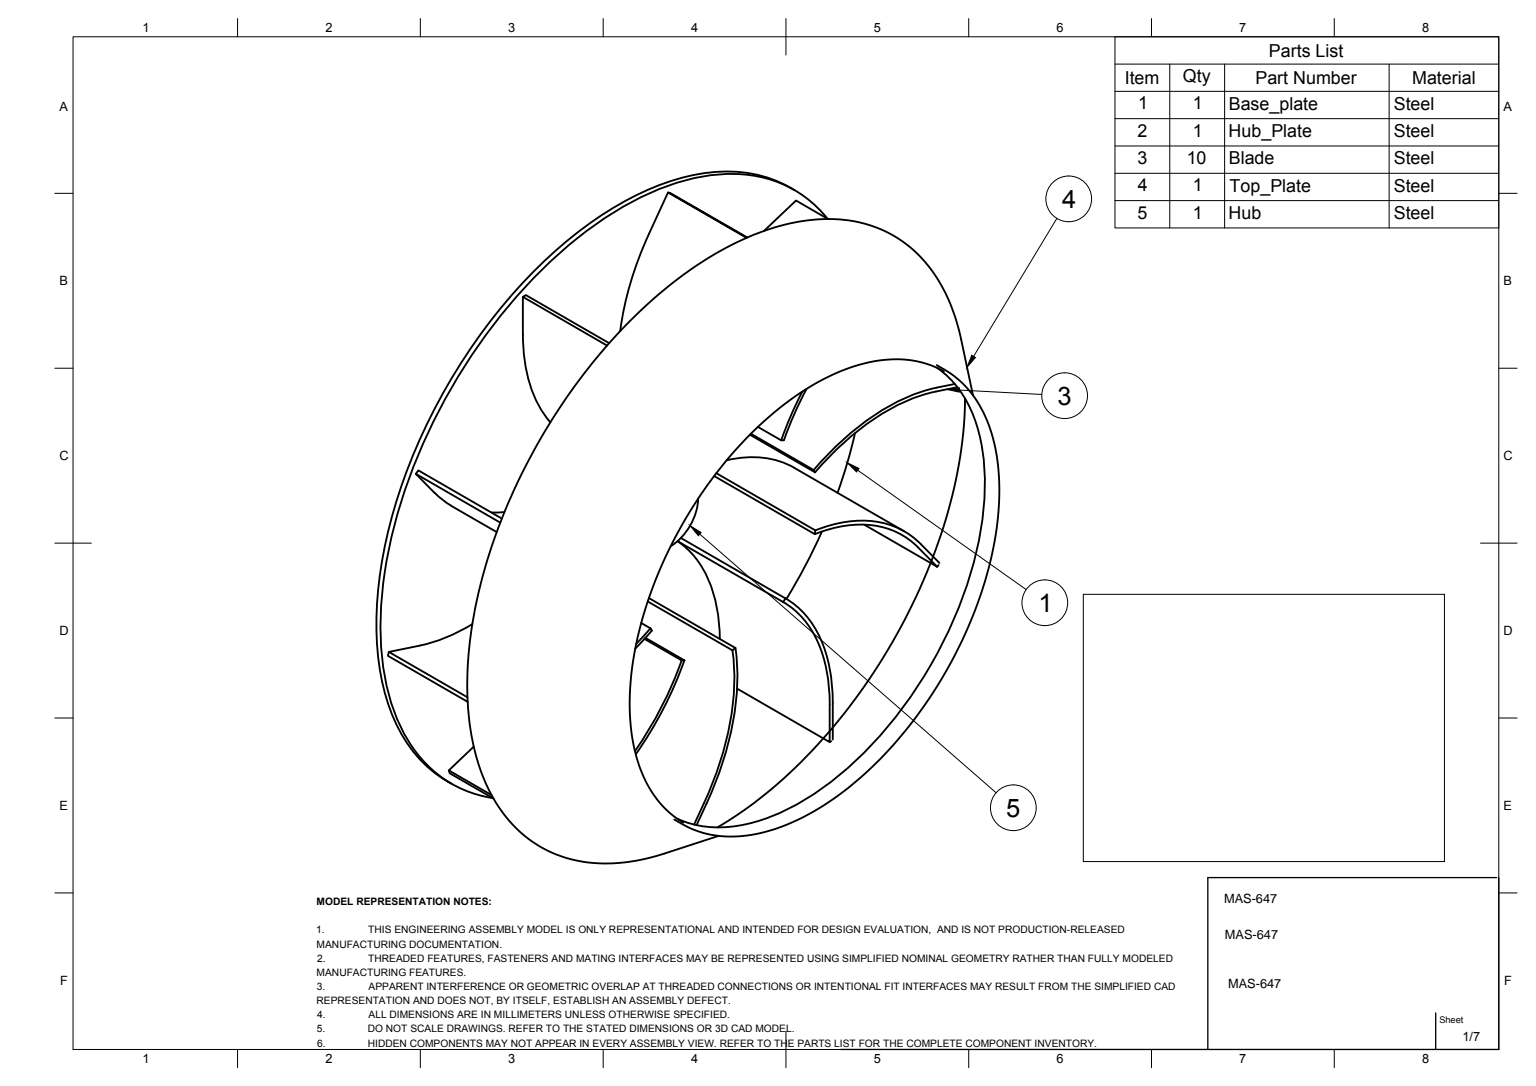
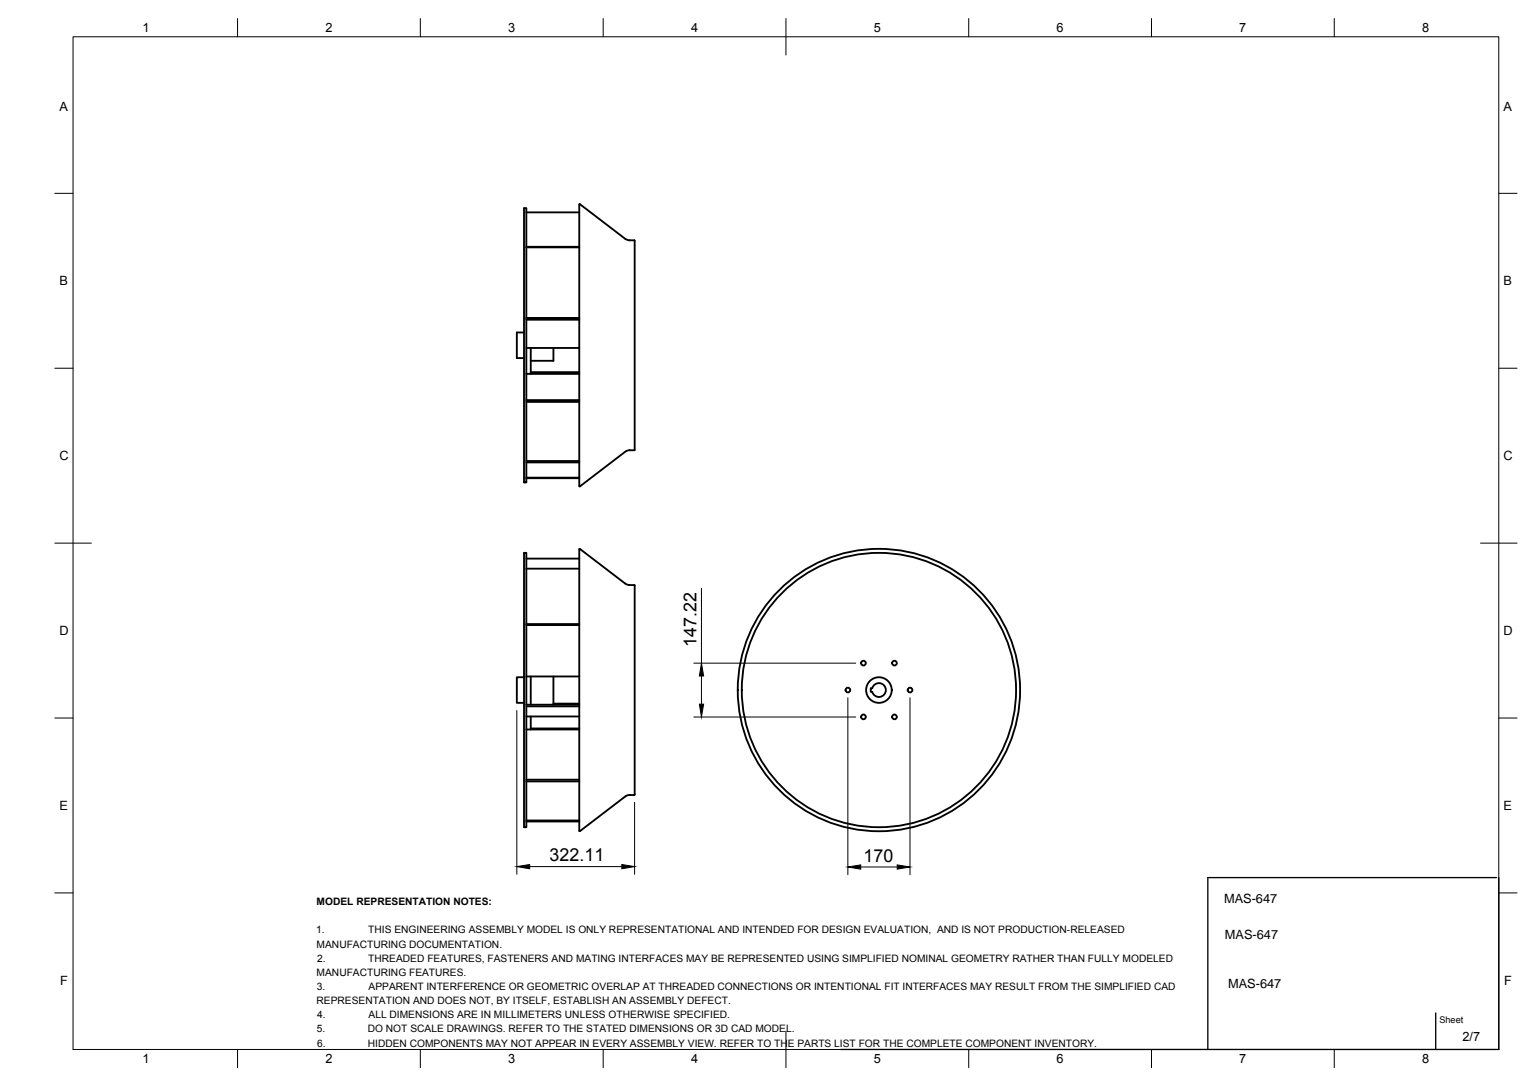
ISO-10303-21;
HEADER;
FILE_DESCRIPTION((''),'2;1');
FILE_NAME('MAS-647','2026-10-09T11:36:02-07:00',(''),(''),'','','');
FILE_SCHEMA (('AUTOMOTIVE_DESIGN { 1 0 10303 214 3 1 1 }'));
ENDSEC;
DATA;
#10 = MECHANICAL_DESIGN_GEOMETRIC_PRESENTATION_REPRESENTATION('',(#82,#83,
#84,#85,#86),#1549) ;
#11 = ITEM_DEFINED_TRANSFORMATION($,$,#906,#1009) ;
#12 = ITEM_DEFINED_TRANSFORMATION($,$,#933,#1010) ;
#13 = ITEM_DEFINED_TRANSFORMATION($,$,#994,#1011) ;
#14 = ITEM_DEFINED_TRANSFORMATION($,$,#960,#1012) ;
#15 = ITEM_DEFINED_TRANSFORMATION($,$,#978,#1013) ;
#16 = ITEM_DEFINED_TRANSFORMATION($,$,#994,#1014) ;
#17 = ITEM_DEFINED_TRANSFORMATION($,$,#994,#1015) ;
#18 = ITEM_DEFINED_TRANSFORMATION($,$,#994,#1016) ;
#19 = ITEM_DEFINED_TRANSFORMATION($,$,#994,#1017) ;
#20 = ITEM_DEFINED_TRANSFORMATION($,$,#994,#1018) ;
#21 = ITEM_DEFINED_TRANSFORMATION($,$,#994,#1019) ;
#22 = ITEM_DEFINED_TRANSFORMATION($,$,#994,#1020) ;
#23 = ITEM_DEFINED_TRANSFORMATION($,$,#994,#1021) ;
#24 = ITEM_DEFINED_TRANSFORMATION($,$,#994,#1022) ;
#25 = (
REPRESENTATION_RELATIONSHIP($,$,#1581,#1580)
REPRESENTATION_RELATIONSHIP_WITH_TRANSFORMATION(#11)
SHAPE_REPRESENTATION_RELATIONSHIP()
) ;
#26 = (
REPRESENTATION_RELATIONSHIP($,$,#1582,#1580)
REPRESENTATION_RELATIONSHIP_WITH_TRANSFORMATION(#12)
SHAPE_REPRESENTATION_RELATIONSHIP()
) ;
#27 = (
REPRESENTATION_RELATIONSHIP($,$,#1585,#1580)
REPRESENTATION_RELATIONSHIP_WITH_TRANSFORMATION(#13)
SHAPE_REPRESENTATION_RELATIONSHIP()
) ;
#28 = (
REPRESENTATION_RELATIONSHIP($,$,#1583,#1580)
REPRESENTATION_RELATIONSHIP_WITH_TRANSFORMATION(#14)
SHAPE_REPRESENTATION_RELATIONSHIP()
) ;
#29 = (
REPRESENTATION_RELATIONSHIP($,$,#1584,#1580)
REPRESENTATION_RELATIONSHIP_WITH_TRANSFORMATION(#15)
SHAPE_REPRESENTATION_RELATIONSHIP()
) ;
#30 = (
REPRESENTATION_RELATIONSHIP($,$,#1585,#1580)
REPRESENTATION_RELATIONSHIP_WITH_TRANSFORMATION(#16)
SHAPE_REPRESENTATION_RELATIONSHIP()
) ;
#31 = (
REPRESENTATION_RELATIONSHIP($,$,#1585,#1580)
REPRESENTATION_RELATIONSHIP_WITH_TRANSFORMATION(#17)
SHAPE_REPRESENTATION_RELATIONSHIP()
) ;
#32 = (
REPRESENTATION_RELATIONSHIP($,$,#1585,#1580)
REPRESENTATION_RELATIONSHIP_WITH_TRANSFORMATION(#18)
SHAPE_REPRESENTATION_RELATIONSHIP()
) ;
#33 = (
REPRESENTATION_RELATIONSHIP($,$,#1585,#1580)
REPRESENTATION_RELATIONSHIP_WITH_TRANSFORMATION(#19)
SHAPE_REPRESENTATION_RELATIONSHIP()
) ;
#34 = (
REPRESENTATION_RELATIONSHIP($,$,#1585,#1580)
REPRESENTATION_RELATIONSHIP_WITH_TRANSFORMATION(#20)
SHAPE_REPRESENTATION_RELATIONSHIP()
) ;
#35 = (
REPRESENTATION_RELATIONSHIP($,$,#1585,#1580)
REPRESENTATION_RELATIONSHIP_WITH_TRANSFORMATION(#21)
SHAPE_REPRESENTATION_RELATIONSHIP()
) ;
#36 = (
REPRESENTATION_RELATIONSHIP($,$,#1585,#1580)
REPRESENTATION_RELATIONSHIP_WITH_TRANSFORMATION(#22)
SHAPE_REPRESENTATION_RELATIONSHIP()
) ;
#37 = (
REPRESENTATION_RELATIONSHIP($,$,#1585,#1580)
REPRESENTATION_RELATIONSHIP_WITH_TRANSFORMATION(#23)
SHAPE_REPRESENTATION_RELATIONSHIP()
) ;
#38 = (
REPRESENTATION_RELATIONSHIP($,$,#1585,#1580)
REPRESENTATION_RELATIONSHIP_WITH_TRANSFORMATION(#24)
SHAPE_REPRESENTATION_RELATIONSHIP()
) ;
#39 = CONTEXT_DEPENDENT_SHAPE_REPRESENTATION(#25,#1566) ;
#40 = CONTEXT_DEPENDENT_SHAPE_REPRESENTATION(#26,#1567) ;
#41 = CONTEXT_DEPENDENT_SHAPE_REPRESENTATION(#27,#1568) ;
#42 = CONTEXT_DEPENDENT_SHAPE_REPRESENTATION(#28,#1569) ;
#43 = CONTEXT_DEPENDENT_SHAPE_REPRESENTATION(#29,#1570) ;
#44 = CONTEXT_DEPENDENT_SHAPE_REPRESENTATION(#30,#1571) ;
#45 = CONTEXT_DEPENDENT_SHAPE_REPRESENTATION(#31,#1572) ;
#46 = CONTEXT_DEPENDENT_SHAPE_REPRESENTATION(#32,#1573) ;
#47 = CONTEXT_DEPENDENT_SHAPE_REPRESENTATION(#33,#1574) ;
#48 = CONTEXT_DEPENDENT_SHAPE_REPRESENTATION(#34,#1575) ;
#49 = CONTEXT_DEPENDENT_SHAPE_REPRESENTATION(#35,#1576) ;
#50 = CONTEXT_DEPENDENT_SHAPE_REPRESENTATION(#36,#1577) ;
#51 = CONTEXT_DEPENDENT_SHAPE_REPRESENTATION(#37,#1578) ;
#52 = CONTEXT_DEPENDENT_SHAPE_REPRESENTATION(#38,#1579) ;
#53 = NEXT_ASSEMBLY_USAGE_OCCURRENCE('Base_Plate:1','Base_Plate:1',
'Base_Plate:1',#1587,#1588,'Base_Plate:1') ;
#54 = NEXT_ASSEMBLY_USAGE_OCCURRENCE('Hub_Plate:1','Hub_Plate:1',
'Hub_Plate:1',#1587,#1589,'Hub_Plate:1') ;
#55 = NEXT_ASSEMBLY_USAGE_OCCURRENCE('Blade:1','Blade:1','Blade:1',#1587,
#1592,'Blade:1') ;
#56 = NEXT_ASSEMBLY_USAGE_OCCURRENCE('Top_Plate:1','Top_Plate:1',
'Top_Plate:1',#1587,#1590,'Top_Plate:1') ;
#57 = NEXT_ASSEMBLY_USAGE_OCCURRENCE('Hub:1','Hub:1','Hub:1',#1587,#1591,
'Hub:1') ;
#58 = NEXT_ASSEMBLY_USAGE_OCCURRENCE('Blade:2','Blade:2','Blade:2',#1587,
#1592,'Blade:2') ;
#59 = NEXT_ASSEMBLY_USAGE_OCCURRENCE('Blade:3','Blade:3','Blade:3',#1587,
#1592,'Blade:3') ;
#60 = NEXT_ASSEMBLY_USAGE_OCCURRENCE('Blade:4','Blade:4','Blade:4',#1587,
#1592,'Blade:4') ;
#61 = NEXT_ASSEMBLY_USAGE_OCCURRENCE('Blade:5','Blade:5','Blade:5',#1587,
#1592,'Blade:5') ;
#62 = NEXT_ASSEMBLY_USAGE_OCCURRENCE('Blade:6','Blade:6','Blade:6',#1587,
#1592,'Blade:6') ;
#63 = NEXT_ASSEMBLY_USAGE_OCCURRENCE('Blade:7','Blade:7','Blade:7',#1587,
#1592,'Blade:7') ;
#64 = NEXT_ASSEMBLY_USAGE_OCCURRENCE('Blade:8','Blade:8','Blade:8',#1587,
#1592,'Blade:8') ;
#65 = NEXT_ASSEMBLY_USAGE_OCCURRENCE('Blade:9','Blade:9','Blade:9',#1587,
#1592,'Blade:9') ;
#66 = NEXT_ASSEMBLY_USAGE_OCCURRENCE('Blade:10','Blade:10','Blade:10',#1587,
#1592,'Blade:10') ;
#67 = CONICAL_SURFACE('',#965,384.29203539823,0.652265221120532) ;
#68 = CONICAL_SURFACE('',#974,287.,0.652265221120532) ;
#69 = TOROIDAL_SURFACE('',#961,307.,20.) ;
#70 = TOROIDAL_SURFACE('',#970,286.,1.) ;
#71 = TOROIDAL_SURFACE('',#976,385.086746274481,0.99999999999999) ;
#72 = SHAPE_REPRESENTATION_RELATIONSHIP('SRR','None',#1581,#77) ;
#73 = SHAPE_REPRESENTATION_RELATIONSHIP('SRR','None',#1582,#78) ;
#74 = SHAPE_REPRESENTATION_RELATIONSHIP('SRR','None',#1583,#79) ;
#75 = SHAPE_REPRESENTATION_RELATIONSHIP('SRR','None',#1584,#80) ;
#76 = SHAPE_REPRESENTATION_RELATIONSHIP('SRR','None',#1585,#81) ;
#77 = ADVANCED_BREP_SHAPE_REPRESENTATION('',(#87),#1544) ;
#78 = ADVANCED_BREP_SHAPE_REPRESENTATION('',(#88),#1545) ;
#79 = ADVANCED_BREP_SHAPE_REPRESENTATION('',(#89),#1546) ;
#80 = ADVANCED_BREP_SHAPE_REPRESENTATION('',(#90),#1547) ;
#81 = ADVANCED_BREP_SHAPE_REPRESENTATION('',(#91),#1548) ;
#82 = STYLED_ITEM('',(#1615),#87) ;
#83 = STYLED_ITEM('',(#1615),#88) ;
#84 = STYLED_ITEM('',(#1615),#89) ;
#85 = STYLED_ITEM('',(#1615),#90) ;
#86 = STYLED_ITEM('',(#1615),#91) ;
#87 = MANIFOLD_SOLID_BREP('Body1',#844) ;
#88 = MANIFOLD_SOLID_BREP('Body1',#845) ;
#89 = MANIFOLD_SOLID_BREP('Body1',#846) ;
#90 = MANIFOLD_SOLID_BREP('Body1',#847) ;
#91 = MANIFOLD_SOLID_BREP('Body1',#848) ;
#92 = FACE_BOUND('',#196,.T.) ;
#93 = FACE_BOUND('',#197,.T.) ;
#94 = FACE_BOUND('',#198,.T.) ;
#95 = FACE_BOUND('',#199,.T.) ;
#96 = FACE_BOUND('',#200,.T.) ;
#97 = FACE_BOUND('',#201,.T.) ;
#98 = FACE_BOUND('',#202,.T.) ;
#99 = FACE_BOUND('',#204,.T.) ;
#100 = FACE_BOUND('',#205,.T.) ;
#101 = FACE_BOUND('',#206,.T.) ;
#102 = FACE_BOUND('',#207,.T.) ;
#103 = FACE_BOUND('',#208,.T.) ;
#104 = FACE_BOUND('',#209,.T.) ;
#105 = FACE_BOUND('',#210,.T.) ;
#106 = FACE_BOUND('',#220,.T.) ;
#107 = FACE_BOUND('',#221,.T.) ;
#108 = FACE_BOUND('',#222,.T.) ;
#109 = FACE_BOUND('',#223,.T.) ;
#110 = FACE_BOUND('',#224,.T.) ;
#111 = FACE_BOUND('',#225,.T.) ;
#112 = FACE_BOUND('',#226,.T.) ;
#113 = FACE_BOUND('',#228,.T.) ;
#114 = FACE_BOUND('',#229,.T.) ;
#115 = FACE_BOUND('',#230,.T.) ;
#116 = FACE_BOUND('',#231,.T.) ;
#117 = FACE_BOUND('',#232,.T.) ;
#118 = FACE_BOUND('',#233,.T.) ;
#119 = FACE_BOUND('',#234,.T.) ;
#120 = FACE_BOUND('',#246,.T.) ;
#121 = FACE_BOUND('',#248,.T.) ;
#122 = FACE_BOUND('',#250,.T.) ;
#123 = PLANE('',#931) ;
#124 = PLANE('',#932) ;
#125 = PLANE('',#958) ;
#126 = PLANE('',#959) ;
#127 = PLANE('',#988) ;
#128 = PLANE('',#989) ;
#129 = PLANE('',#990) ;
#130 = PLANE('',#991) ;
#131 = PLANE('',#992) ;
#132 = PLANE('',#993) ;
#133 = PLANE('',#995) ;
#134 = PLANE('',#998) ;
#135 = PLANE('',#1001) ;
#136 = PLANE('',#1002) ;
#137 = PLANE('',#1003) ;
#138 = PLANE('',#1005) ;
#139 = PLANE('',#1007) ;
#140 = PLANE('',#1008) ;
#141 = FACE_OUTER_BOUND('',#187,.T.) ;
#142 = FACE_OUTER_BOUND('',#188,.T.) ;
#143 = FACE_OUTER_BOUND('',#189,.T.) ;
#144 = FACE_OUTER_BOUND('',#190,.T.) ;
#145 = FACE_OUTER_BOUND('',#191,.T.) ;
#146 = FACE_OUTER_BOUND('',#192,.T.) ;
#147 = FACE_OUTER_BOUND('',#193,.T.) ;
#148 = FACE_OUTER_BOUND('',#194,.T.) ;
#149 = FACE_OUTER_BOUND('',#195,.T.) ;
#150 = FACE_OUTER_BOUND('',#203,.T.) ;
#151 = FACE_OUTER_BOUND('',#211,.T.) ;
#152 = FACE_OUTER_BOUND('',#212,.T.) ;
#153 = FACE_OUTER_BOUND('',#213,.T.) ;
#154 = FACE_OUTER_BOUND('',#214,.T.) ;
#155 = FACE_OUTER_BOUND('',#215,.T.) ;
#156 = FACE_OUTER_BOUND('',#216,.T.) ;
#157 = FACE_OUTER_BOUND('',#217,.T.) ;
#158 = FACE_OUTER_BOUND('',#218,.T.) ;
#159 = FACE_OUTER_BOUND('',#219,.T.) ;
#160 = FACE_OUTER_BOUND('',#227,.T.) ;
#161 = FACE_OUTER_BOUND('',#235,.T.) ;
#162 = FACE_OUTER_BOUND('',#236,.T.) ;
#163 = FACE_OUTER_BOUND('',#237,.T.) ;
#164 = FACE_OUTER_BOUND('',#238,.T.) ;
#165 = FACE_OUTER_BOUND('',#239,.T.) ;
#166 = FACE_OUTER_BOUND('',#240,.T.) ;
#167 = FACE_OUTER_BOUND('',#241,.T.) ;
#168 = FACE_OUTER_BOUND('',#242,.T.) ;
#169 = FACE_OUTER_BOUND('',#243,.T.) ;
#170 = FACE_OUTER_BOUND('',#244,.T.) ;
#171 = FACE_OUTER_BOUND('',#245,.T.) ;
#172 = FACE_OUTER_BOUND('',#247,.T.) ;
#173 = FACE_OUTER_BOUND('',#249,.T.) ;
#174 = FACE_OUTER_BOUND('',#251,.T.) ;
#175 = FACE_OUTER_BOUND('',#252,.T.) ;
#176 = FACE_OUTER_BOUND('',#253,.T.) ;
#177 = FACE_OUTER_BOUND('',#254,.T.) ;
#178 = FACE_OUTER_BOUND('',#255,.T.) ;
#179 = FACE_OUTER_BOUND('',#256,.T.) ;
#180 = FACE_OUTER_BOUND('',#257,.T.) ;
#181 = FACE_OUTER_BOUND('',#258,.T.) ;
#182 = FACE_OUTER_BOUND('',#259,.T.) ;
#183 = FACE_OUTER_BOUND('',#260,.T.) ;
#184 = FACE_OUTER_BOUND('',#261,.T.) ;
#185 = FACE_OUTER_BOUND('',#262,.T.) ;
#186 = FACE_OUTER_BOUND('',#263,.T.) ;
#187 = EDGE_LOOP('',(#575,#576,#577,#578)) ;
#188 = EDGE_LOOP('',(#579,#580,#581,#582)) ;
#189 = EDGE_LOOP('',(#583,#584,#585,#586)) ;
#190 = EDGE_LOOP('',(#587,#588,#589,#590)) ;
#191 = EDGE_LOOP('',(#591,#592,#593,#594)) ;
#192 = EDGE_LOOP('',(#595,#596,#597,#598)) ;
#193 = EDGE_LOOP('',(#599,#600,#601,#602)) ;
#194 = EDGE_LOOP('',(#603,#604,#605,#606)) ;
#195 = EDGE_LOOP('',(#607)) ;
#196 = EDGE_LOOP('',(#608)) ;
#197 = EDGE_LOOP('',(#609)) ;
#198 = EDGE_LOOP('',(#610)) ;
#199 = EDGE_LOOP('',(#611)) ;
#200 = EDGE_LOOP('',(#612)) ;
#201 = EDGE_LOOP('',(#613)) ;
#202 = EDGE_LOOP('',(#614)) ;
#203 = EDGE_LOOP('',(#615)) ;
#204 = EDGE_LOOP('',(#616)) ;
#205 = EDGE_LOOP('',(#617)) ;
#206 = EDGE_LOOP('',(#618)) ;
#207 = EDGE_LOOP('',(#619)) ;
#208 = EDGE_LOOP('',(#620)) ;
#209 = EDGE_LOOP('',(#621)) ;
#210 = EDGE_LOOP('',(#622)) ;
#211 = EDGE_LOOP('',(#623,#624,#625,#626)) ;
#212 = EDGE_LOOP('',(#627,#628,#629,#630)) ;
#213 = EDGE_LOOP('',(#631,#632,#633,#634)) ;
#214 = EDGE_LOOP('',(#635,#636,#637,#638)) ;
#215 = EDGE_LOOP('',(#639,#640,#641,#642)) ;
#216 = EDGE_LOOP('',(#643,#644,#645,#646)) ;
#217 = EDGE_LOOP('',(#647,#648,#649,#650)) ;
#218 = EDGE_LOOP('',(#651,#652,#653,#654)) ;
#219 = EDGE_LOOP('',(#655)) ;
#220 = EDGE_LOOP('',(#656)) ;
#221 = EDGE_LOOP('',(#657)) ;
#222 = EDGE_LOOP('',(#658)) ;
#223 = EDGE_LOOP('',(#659)) ;
#224 = EDGE_LOOP('',(#660)) ;
#225 = EDGE_LOOP('',(#661)) ;
#226 = EDGE_LOOP('',(#662)) ;
#227 = EDGE_LOOP('',(#663)) ;
#228 = EDGE_LOOP('',(#664)) ;
#229 = EDGE_LOOP('',(#665)) ;
#230 = EDGE_LOOP('',(#666)) ;
#231 = EDGE_LOOP('',(#667)) ;
#232 = EDGE_LOOP('',(#668)) ;
#233 = EDGE_LOOP('',(#669)) ;
#234 = EDGE_LOOP('',(#670)) ;
#235 = EDGE_LOOP('',(#671,#672,#673,#674)) ;
#236 = EDGE_LOOP('',(#675,#676,#677,#678)) ;
#237 = EDGE_LOOP('',(#679,#680,#681,#682)) ;
#238 = EDGE_LOOP('',(#683,#684,#685,#686)) ;
#239 = EDGE_LOOP('',(#687,#688,#689,#690)) ;
#240 = EDGE_LOOP('',(#691,#692,#693,#694)) ;
#241 = EDGE_LOOP('',(#695,#696,#697,#698)) ;
#242 = EDGE_LOOP('',(#699,#700,#701,#702)) ;
#243 = EDGE_LOOP('',(#703,#704,#705,#706)) ;
#244 = EDGE_LOOP('',(#707,#708,#709,#710)) ;
#245 = EDGE_LOOP('',(#711)) ;
#246 = EDGE_LOOP('',(#712,#713,#714,#715)) ;
#247 = EDGE_LOOP('',(#716)) ;
#248 = EDGE_LOOP('',(#717)) ;
#249 = EDGE_LOOP('',(#718)) ;
#250 = EDGE_LOOP('',(#719,#720,#721,#722)) ;
#251 = EDGE_LOOP('',(#723,#724,#725,#726)) ;
#252 = EDGE_LOOP('',(#727,#728,#729,#730)) ;
#253 = EDGE_LOOP('',(#731,#732,#733,#734)) ;
#254 = EDGE_LOOP('',(#735,#736,#737,#738)) ;
#255 = EDGE_LOOP('',(#739,#740,#741,#742)) ;
#256 = EDGE_LOOP('',(#743,#744,#745,#746)) ;
#257 = EDGE_LOOP('',(#747,#748,#749,#750)) ;
#258 = EDGE_LOOP('',(#751,#752,#753,#754)) ;
#259 = EDGE_LOOP('',(#755,#756,#757,#758)) ;
#260 = EDGE_LOOP('',(#759,#760,#761,#762)) ;
#261 = EDGE_LOOP('',(#763,#764,#765,#766)) ;
#262 = EDGE_LOOP('',(#767,#768,#769,#770)) ;
#263 = EDGE_LOOP('',(#771,#772,#773,#774)) ;
#264 = LINE('',#1313,#312) ;
#265 = LINE('',#1319,#313) ;
#266 = LINE('',#1325,#314) ;
#267 = LINE('',#1331,#315) ;
#268 = LINE('',#1337,#316) ;
#269 = LINE('',#1343,#317) ;
#270 = LINE('',#1349,#318) ;
#271 = LINE('',#1355,#319) ;
#272 = LINE('',#1364,#320) ;
#273 = LINE('',#1370,#321) ;
#274 = LINE('',#1376,#322) ;
#275 = LINE('',#1382,#323) ;
#276 = LINE('',#1388,#324) ;
#277 = LINE('',#1394,#325) ;
#278 = LINE('',#1400,#326) ;
#279 = LINE('',#1406,#327) ;
#280 = LINE('',#1421,#328) ;
#281 = LINE('',#1426,#329) ;
#282 = LINE('',#1432,#330) ;
#283 = LINE('',#1436,#331) ;
#284 = LINE('',#1444,#332) ;
#285 = LINE('',#1450,#333) ;
#286 = LINE('',#1457,#334) ;
#287 = LINE('',#1460,#335) ;
#288 = LINE('',#1464,#336) ;
#289 = LINE('',#1465,#337) ;
#290 = LINE('',#1466,#338) ;
#291 = LINE('',#1470,#339) ;
#292 = LINE('',#1472,#340) ;
#293 = LINE('',#1473,#341) ;
#294 = LINE('',#1475,#342) ;
#295 = LINE('',#1477,#343) ;
#296 = LINE('',#1483,#344) ;
#297 = LINE('',#1487,#345) ;
#298 = LINE('',#1492,#346) ;
#299 = LINE('',#1496,#347) ;
#300 = LINE('',#1500,#348) ;
#301 = LINE('',#1502,#349) ;
#302 = LINE('',#1503,#350) ;
#303 = LINE('',#1504,#351) ;
#304 = LINE('',#1507,#352) ;
#305 = LINE('',#1509,#353) ;
#306 = LINE('',#1510,#354) ;
#307 = LINE('',#1512,#355) ;
#308 = LINE('',#1513,#356) ;
#309 = LINE('',#1514,#357) ;
#310 = LINE('',#1516,#358) ;
#311 = LINE('',#1518,#359) ;
#312 = VECTOR('',#1031,6.49999999999999) ;
#313 = VECTOR('',#1038,6.49999999999999) ;
#314 = VECTOR('',#1045,6.49999999999999) ;
#315 = VECTOR('',#1052,6.49999999999999) ;
#316 = VECTOR('',#1059,6.49999999999999) ;
#317 = VECTOR('',#1066,6.49999999999999) ;
#318 = VECTOR('',#1073,35.) ;
#319 = VECTOR('',#1080,375.) ;
#320 = VECTOR('',#1093,6.49999999999999) ;
#321 = VECTOR('',#1100,6.49999999999999) ;
#322 = VECTOR('',#1107,6.49999999999999) ;
#323 = VECTOR('',#1114,6.49999999999999) ;
#324 = VECTOR('',#1121,6.49999999999999) ;
#325 = VECTOR('',#1128,6.49999999999999) ;
#326 = VECTOR('',#1135,35.) ;
#327 = VECTOR('',#1142,120.) ;
#328 = VECTOR('',#1163,384.29203539823) ;
#329 = VECTOR('',#1170,285.) ;
#330 = VECTOR('',#1179,287.) ;
#331 = VECTOR('',#1184,287.) ;
#332 = VECTOR('',#1195,42.5) ;
#333 = VECTOR('',#1202,35.) ;
#334 = VECTOR('',#1209,1000.) ;
#335 = VECTOR('',#1212,1000.) ;
#336 = VECTOR('',#1215,1000.) ;
#337 = VECTOR('',#1216,1000.) ;
#338 = VECTOR('',#1217,1000.) ;
#339 = VECTOR('',#1222,1000.) ;
#340 = VECTOR('',#1223,1000.) ;
#341 = VECTOR('',#1224,1000.) ;
#342 = VECTOR('',#1227,1000.) ;
#343 = VECTOR('',#1230,1000.) ;
#344 = VECTOR('',#1237,1000.) ;
#345 = VECTOR('',#1240,1000.) ;
#346 = VECTOR('',#1245,1000.) ;
#347 = VECTOR('',#1248,1000.) ;
#348 = VECTOR('',#1253,1000.) ;
#349 = VECTOR('',#1254,1000.) ;
#350 = VECTOR('',#1255,1000.) ;
#351 = VECTOR('',#1256,1000.) ;
#352 = VECTOR('',#1259,1000.) ;
#353 = VECTOR('',#1260,1000.) ;
#354 = VECTOR('',#1261,1000.) ;
#355 = VECTOR('',#1264,1000.) ;
#356 = VECTOR('',#1265,1000.) ;
#357 = VECTOR('',#1266,1000.) ;
#358 = VECTOR('',#1269,1000.) ;
#359 = VECTOR('',#1272,1000.) ;
#360 = CIRCLE('',#908,6.49999999999999) ;
#361 = CIRCLE('',#909,6.49999999999999) ;
#362 = CIRCLE('',#911,6.49999999999999) ;
#363 = CIRCLE('',#912,6.49999999999998) ;
#364 = CIRCLE('',#914,6.49999999999999) ;
#365 = CIRCLE('',#915,6.49999999999999) ;
#366 = CIRCLE('',#917,6.49999999999999) ;
#367 = CIRCLE('',#918,6.49999999999999) ;
#368 = CIRCLE('',#920,6.49999999999999) ;
#369 = CIRCLE('',#921,6.49999999999999) ;
#370 = CIRCLE('',#923,6.49999999999999) ;
#371 = CIRCLE('',#924,6.49999999999999) ;
#372 = CIRCLE('',#926,35.) ;
#373 = CIRCLE('',#927,35.) ;
#374 = CIRCLE('',#929,375.) ;
#375 = CIRCLE('',#930,375.) ;
#376 = CIRCLE('',#935,6.49999999999999) ;
#377 = CIRCLE('',#936,6.49999999999999) ;
#378 = CIRCLE('',#938,6.49999999999999) ;
#379 = CIRCLE('',#939,6.49999999999998) ;
#380 = CIRCLE('',#941,6.49999999999999) ;
#381 = CIRCLE('',#942,6.49999999999999) ;
#382 = CIRCLE('',#944,6.49999999999999) ;
#383 = CIRCLE('',#945,6.49999999999999) ;
#384 = CIRCLE('',#947,6.49999999999999) ;
#385 = CIRCLE('',#948,6.49999999999999) ;
#386 = CIRCLE('',#950,6.49999999999999) ;
#387 = CIRCLE('',#951,6.49999999999999) ;
#388 = CIRCLE('',#953,35.) ;
#389 = CIRCLE('',#954,35.) ;
#390 = CIRCLE('',#956,120.) ;
#391 = CIRCLE('',#957,120.) ;
#392 = CIRCLE('',#962,291.105782474981) ;
#393 = CIRCLE('',#963,20.) ;
#394 = CIRCLE('',#964,287.) ;
#395 = CIRCLE('',#966,285.) ;
#396 = CIRCLE('',#967,384.29203539823) ;
#397 = CIRCLE('',#969,285.) ;
#398 = CIRCLE('',#971,287.) ;
#399 = CIRCLE('',#972,1.) ;
#400 = CIRCLE('',#975,385.881457150732) ;
#401 = CIRCLE('',#977,0.99999999999999) ;
#402 = CIRCLE('',#980,42.5) ;
#403 = CIRCLE('',#981,42.5) ;
#404 = CIRCLE('',#983,35.) ;
#405 = CIRCLE('',#984,35.) ;
#406 = CIRCLE('',#986,19.) ;
#407 = CIRCLE('',#987,19.) ;
#408 = CIRCLE('',#996,250.) ;
#409 = CIRCLE('',#997,245.24) ;
#410 = CIRCLE('',#999,245.24) ;
#411 = CIRCLE('',#1000,250.) ;
#412 = VERTEX_POINT('',#1310) ;
#413 = VERTEX_POINT('',#1312) ;
#414 = VERTEX_POINT('',#1316) ;
#415 = VERTEX_POINT('',#1318) ;
#416 = VERTEX_POINT('',#1322) ;
#417 = VERTEX_POINT('',#1324) ;
#418 = VERTEX_POINT('',#1328) ;
#419 = VERTEX_POINT('',#1330) ;
#420 = VERTEX_POINT('',#1334) ;
#421 = VERTEX_POINT('',#1336) ;
#422 = VERTEX_POINT('',#1340) ;
#423 = VERTEX_POINT('',#1342) ;
#424 = VERTEX_POINT('',#1346) ;
#425 = VERTEX_POINT('',#1348) ;
#426 = VERTEX_POINT('',#1352) ;
#427 = VERTEX_POINT('',#1354) ;
#428 = VERTEX_POINT('',#1361) ;
#429 = VERTEX_POINT('',#1363) ;
#430 = VERTEX_POINT('',#1367) ;
#431 = VERTEX_POINT('',#1369) ;
#432 = VERTEX_POINT('',#1373) ;
#433 = VERTEX_POINT('',#1375) ;
#434 = VERTEX_POINT('',#1379) ;
#435 = VERTEX_POINT('',#1381) ;
#436 = VERTEX_POINT('',#1385) ;
#437 = VERTEX_POINT('',#1387) ;
#438 = VERTEX_POINT('',#1391) ;
#439 = VERTEX_POINT('',#1393) ;
#440 = VERTEX_POINT('',#1397) ;
#441 = VERTEX_POINT('',#1399) ;
#442 = VERTEX_POINT('',#1403) ;
#443 = VERTEX_POINT('',#1405) ;
#444 = VERTEX_POINT('',#1412) ;
#445 = VERTEX_POINT('',#1414) ;
#446 = VERTEX_POINT('',#1418) ;
#447 = VERTEX_POINT('',#1420) ;
#448 = VERTEX_POINT('',#1424) ;
#449 = VERTEX_POINT('',#1428) ;
#450 = VERTEX_POINT('',#1434) ;
#451 = VERTEX_POINT('',#1441) ;
#452 = VERTEX_POINT('',#1443) ;
#453 = VERTEX_POINT('',#1447) ;
#454 = VERTEX_POINT('',#1449) ;
#455 = VERTEX_POINT('',#1453) ;
#456 = VERTEX_POINT('',#1454) ;
#457 = VERTEX_POINT('',#1456) ;
#458 = VERTEX_POINT('',#1458) ;
#459 = VERTEX_POINT('',#1462) ;
#460 = VERTEX_POINT('',#1463) ;
#461 = VERTEX_POINT('',#1469) ;
#462 = VERTEX_POINT('',#1471) ;
#463 = VERTEX_POINT('',#1481) ;
#464 = VERTEX_POINT('',#1482) ;
#465 = VERTEX_POINT('',#1484) ;
#466 = VERTEX_POINT('',#1486) ;
#467 = VERTEX_POINT('',#1490) ;
#468 = VERTEX_POINT('',#1491) ;
#469 = VERTEX_POINT('',#1493) ;
#470 = VERTEX_POINT('',#1495) ;
#471 = VERTEX_POINT('',#1499) ;
#472 = VERTEX_POINT('',#1501) ;
#473 = VERTEX_POINT('',#1506) ;
#474 = VERTEX_POINT('',#1508) ;
#475 = EDGE_CURVE('',#412,#412,#360,.T.) ;
#476 = EDGE_CURVE('',#412,#413,#264,.T.) ;
#477 = EDGE_CURVE('',#413,#413,#361,.T.) ;
#478 = EDGE_CURVE('',#414,#414,#362,.T.) ;
#479 = EDGE_CURVE('',#414,#415,#265,.T.) ;
#480 = EDGE_CURVE('',#415,#415,#363,.T.) ;
#481 = EDGE_CURVE('',#416,#416,#364,.T.) ;
#482 = EDGE_CURVE('',#416,#417,#266,.T.) ;
#483 = EDGE_CURVE('',#417,#417,#365,.T.) ;
#484 = EDGE_CURVE('',#418,#418,#366,.T.) ;
#485 = EDGE_CURVE('',#418,#419,#267,.T.) ;
#486 = EDGE_CURVE('',#419,#419,#367,.T.) ;
#487 = EDGE_CURVE('',#420,#420,#368,.T.) ;
#488 = EDGE_CURVE('',#420,#421,#268,.T.) ;
#489 = EDGE_CURVE('',#421,#421,#369,.T.) ;
#490 = EDGE_CURVE('',#422,#422,#370,.T.) ;
#491 = EDGE_CURVE('',#422,#423,#269,.T.) ;
#492 = EDGE_CURVE('',#423,#423,#371,.T.) ;
#493 = EDGE_CURVE('',#424,#424,#372,.T.) ;
#494 = EDGE_CURVE('',#424,#425,#270,.T.) ;
#495 = EDGE_CURVE('',#425,#425,#373,.T.) ;
#496 = EDGE_CURVE('',#426,#426,#374,.T.) ;
#497 = EDGE_CURVE('',#426,#427,#271,.T.) ;
#498 = EDGE_CURVE('',#427,#427,#375,.T.) ;
#499 = EDGE_CURVE('',#428,#428,#376,.T.) ;
#500 = EDGE_CURVE('',#428,#429,#272,.T.) ;
#501 = EDGE_CURVE('',#429,#429,#377,.T.) ;
#502 = EDGE_CURVE('',#430,#430,#378,.T.) ;
#503 = EDGE_CURVE('',#430,#431,#273,.T.) ;
#504 = EDGE_CURVE('',#431,#431,#379,.T.) ;
#505 = EDGE_CURVE('',#432,#432,#380,.T.) ;
#506 = EDGE_CURVE('',#432,#433,#274,.T.) ;
#507 = EDGE_CURVE('',#433,#433,#381,.T.) ;
#508 = EDGE_CURVE('',#434,#434,#382,.T.) ;
#509 = EDGE_CURVE('',#434,#435,#275,.T.) ;
#510 = EDGE_CURVE('',#435,#435,#383,.T.) ;
#511 = EDGE_CURVE('',#436,#436,#384,.T.) ;
#512 = EDGE_CURVE('',#436,#437,#276,.T.) ;
#513 = EDGE_CURVE('',#437,#437,#385,.T.) ;
#514 = EDGE_CURVE('',#438,#438,#386,.T.) ;
#515 = EDGE_CURVE('',#438,#439,#277,.T.) ;
#516 = EDGE_CURVE('',#439,#439,#387,.T.) ;
#517 = EDGE_CURVE('',#440,#440,#388,.T.) ;
#518 = EDGE_CURVE('',#440,#441,#278,.T.) ;
#519 = EDGE_CURVE('',#441,#441,#389,.T.) ;
#520 = EDGE_CURVE('',#442,#442,#390,.T.) ;
#521 = EDGE_CURVE('',#442,#443,#279,.T.) ;
#522 = EDGE_CURVE('',#443,#443,#391,.T.) ;
#523 = EDGE_CURVE('',#444,#444,#392,.T.) ;
#524 = EDGE_CURVE('',#444,#445,#393,.T.) ;
#525 = EDGE_CURVE('',#445,#445,#394,.T.) ;
#526 = EDGE_CURVE('',#446,#446,#395,.T.) ;
#527 = EDGE_CURVE('',#446,#447,#280,.T.) ;
#528 = EDGE_CURVE('',#447,#447,#396,.T.) ;
#529 = EDGE_CURVE('',#448,#448,#397,.T.) ;
#530 = EDGE_CURVE('',#448,#446,#281,.T.) ;
#531 = EDGE_CURVE('',#449,#449,#398,.T.) ;
#532 = EDGE_CURVE('',#449,#448,#399,.T.) ;
#533 = EDGE_CURVE('',#445,#449,#282,.T.) ;
#534 = EDGE_CURVE('',#450,#450,#400,.T.) ;
#535 = EDGE_CURVE('',#450,#444,#283,.T.) ;
#536 = EDGE_CURVE('',#447,#450,#401,.T.) ;
#537 = EDGE_CURVE('',#451,#451,#402,.T.) ;
#538 = EDGE_CURVE('',#451,#452,#284,.T.) ;
#539 = EDGE_CURVE('',#452,#452,#403,.T.) ;
#540 = EDGE_CURVE('',#453,#453,#404,.T.) ;
#541 = EDGE_CURVE('',#453,#454,#285,.T.) ;
#542 = EDGE_CURVE('',#454,#454,#405,.T.) ;
#543 = EDGE_CURVE('',#455,#456,#406,.T.) ;
#544 = EDGE_CURVE('',#457,#455,#286,.T.) ;
#545 = EDGE_CURVE('',#457,#458,#407,.T.) ;
#546 = EDGE_CURVE('',#458,#456,#287,.T.) ;
#547 = EDGE_CURVE('',#459,#460,#288,.T.) ;
#548 = EDGE_CURVE('',#460,#458,#289,.T.) ;
#549 = EDGE_CURVE('',#457,#459,#290,.T.) ;
#550 = EDGE_CURVE('',#461,#456,#291,.T.) ;
#551 = EDGE_CURVE('',#462,#461,#292,.T.) ;
#552 = EDGE_CURVE('',#455,#462,#293,.T.) ;
#553 = EDGE_CURVE('',#460,#461,#294,.T.) ;
#554 = EDGE_CURVE('',#459,#462,#295,.T.) ;
#555 = EDGE_CURVE('',#463,#464,#296,.T.) ;
#556 = EDGE_CURVE('',#465,#463,#408,.T.) ;
#557 = EDGE_CURVE('',#466,#465,#297,.T.) ;
#558 = EDGE_CURVE('',#466,#464,#409,.T.) ;
#559 = EDGE_CURVE('',#467,#468,#298,.T.) ;
#560 = EDGE_CURVE('',#469,#467,#410,.T.) ;
#561 = EDGE_CURVE('',#469,#470,#299,.T.) ;
#562 = EDGE_CURVE('',#470,#468,#411,.T.) ;
#563 = EDGE_CURVE('',#467,#471,#300,.T.) ;
#564 = EDGE_CURVE('',#472,#471,#301,.T.) ;
#565 = EDGE_CURVE('',#464,#472,#302,.T.) ;
#566 = EDGE_CURVE('',#464,#467,#303,.T.) ;
#567 = EDGE_CURVE('',#473,#471,#304,.T.) ;
#568 = EDGE_CURVE('',#474,#473,#305,.T.) ;
#569 = EDGE_CURVE('',#474,#472,#306,.T.) ;
#570 = EDGE_CURVE('',#468,#473,#307,.T.) ;
#571 = EDGE_CURVE('',#463,#468,#308,.T.) ;
#572 = EDGE_CURVE('',#463,#474,#309,.T.) ;
#573 = EDGE_CURVE('',#465,#470,#310,.T.) ;
#574 = EDGE_CURVE('',#466,#469,#311,.T.) ;
#575 = ORIENTED_EDGE('',*,*,#475,.F.) ;
#576 = ORIENTED_EDGE('',*,*,#476,.T.) ;
#577 = ORIENTED_EDGE('',*,*,#477,.T.) ;
#578 = ORIENTED_EDGE('',*,*,#476,.F.) ;
#579 = ORIENTED_EDGE('',*,*,#478,.F.) ;
#580 = ORIENTED_EDGE('',*,*,#479,.T.) ;
#581 = ORIENTED_EDGE('',*,*,#480,.T.) ;
#582 = ORIENTED_EDGE('',*,*,#479,.F.) ;
#583 = ORIENTED_EDGE('',*,*,#481,.F.) ;
#584 = ORIENTED_EDGE('',*,*,#482,.T.) ;
#585 = ORIENTED_EDGE('',*,*,#483,.T.) ;
#586 = ORIENTED_EDGE('',*,*,#482,.F.) ;
#587 = ORIENTED_EDGE('',*,*,#484,.F.) ;
#588 = ORIENTED_EDGE('',*,*,#485,.T.) ;
#589 = ORIENTED_EDGE('',*,*,#486,.T.) ;
#590 = ORIENTED_EDGE('',*,*,#485,.F.) ;
#591 = ORIENTED_EDGE('',*,*,#487,.F.) ;
#592 = ORIENTED_EDGE('',*,*,#488,.T.) ;
#593 = ORIENTED_EDGE('',*,*,#489,.T.) ;
#594 = ORIENTED_EDGE('',*,*,#488,.F.) ;
#595 = ORIENTED_EDGE('',*,*,#490,.F.) ;
#596 = ORIENTED_EDGE('',*,*,#491,.T.) ;
#597 = ORIENTED_EDGE('',*,*,#492,.T.) ;
#598 = ORIENTED_EDGE('',*,*,#491,.F.) ;
#599 = ORIENTED_EDGE('',*,*,#493,.F.) ;
#600 = ORIENTED_EDGE('',*,*,#494,.T.) ;
#601 = ORIENTED_EDGE('',*,*,#495,.T.) ;
#602 = ORIENTED_EDGE('',*,*,#494,.F.) ;
#603 = ORIENTED_EDGE('',*,*,#496,.F.) ;
#604 = ORIENTED_EDGE('',*,*,#497,.T.) ;
#605 = ORIENTED_EDGE('',*,*,#498,.T.) ;
#606 = ORIENTED_EDGE('',*,*,#497,.F.) ;
#607 = ORIENTED_EDGE('',*,*,#498,.F.) ;
#608 = ORIENTED_EDGE('',*,*,#475,.T.) ;
#609 = ORIENTED_EDGE('',*,*,#478,.T.) ;
#610 = ORIENTED_EDGE('',*,*,#481,.T.) ;
#611 = ORIENTED_EDGE('',*,*,#484,.T.) ;
#612 = ORIENTED_EDGE('',*,*,#487,.T.) ;
#613 = ORIENTED_EDGE('',*,*,#490,.T.) ;
#614 = ORIENTED_EDGE('',*,*,#493,.T.) ;
#615 = ORIENTED_EDGE('',*,*,#496,.T.) ;
#616 = ORIENTED_EDGE('',*,*,#477,.F.) ;
#617 = ORIENTED_EDGE('',*,*,#480,.F.) ;
#618 = ORIENTED_EDGE('',*,*,#483,.F.) ;
#619 = ORIENTED_EDGE('',*,*,#486,.F.) ;
#620 = ORIENTED_EDGE('',*,*,#489,.F.) ;
#621 = ORIENTED_EDGE('',*,*,#492,.F.) ;
#622 = ORIENTED_EDGE('',*,*,#495,.F.) ;
#623 = ORIENTED_EDGE('',*,*,#499,.F.) ;
#624 = ORIENTED_EDGE('',*,*,#500,.T.) ;
#625 = ORIENTED_EDGE('',*,*,#501,.T.) ;
#626 = ORIENTED_EDGE('',*,*,#500,.F.) ;
#627 = ORIENTED_EDGE('',*,*,#502,.F.) ;
#628 = ORIENTED_EDGE('',*,*,#503,.T.) ;
#629 = ORIENTED_EDGE('',*,*,#504,.T.) ;
#630 = ORIENTED_EDGE('',*,*,#503,.F.) ;
#631 = ORIENTED_EDGE('',*,*,#505,.F.) ;
#632 = ORIENTED_EDGE('',*,*,#506,.T.) ;
#633 = ORIENTED_EDGE('',*,*,#507,.T.) ;
#634 = ORIENTED_EDGE('',*,*,#506,.F.) ;
#635 = ORIENTED_EDGE('',*,*,#508,.F.) ;
#636 = ORIENTED_EDGE('',*,*,#509,.T.) ;
#637 = ORIENTED_EDGE('',*,*,#510,.T.) ;
#638 = ORIENTED_EDGE('',*,*,#509,.F.) ;
#639 = ORIENTED_EDGE('',*,*,#511,.F.) ;
#640 = ORIENTED_EDGE('',*,*,#512,.T.) ;
#641 = ORIENTED_EDGE('',*,*,#513,.T.) ;
#642 = ORIENTED_EDGE('',*,*,#512,.F.) ;
#643 = ORIENTED_EDGE('',*,*,#514,.F.) ;
#644 = ORIENTED_EDGE('',*,*,#515,.T.) ;
#645 = ORIENTED_EDGE('',*,*,#516,.T.) ;
#646 = ORIENTED_EDGE('',*,*,#515,.F.) ;
#647 = ORIENTED_EDGE('',*,*,#517,.T.) ;
#648 = ORIENTED_EDGE('',*,*,#518,.T.) ;
#649 = ORIENTED_EDGE('',*,*,#519,.F.) ;
#650 = ORIENTED_EDGE('',*,*,#518,.F.) ;
#651 = ORIENTED_EDGE('',*,*,#520,.T.) ;
#652 = ORIENTED_EDGE('',*,*,#521,.T.) ;
#653 = ORIENTED_EDGE('',*,*,#522,.F.) ;
#654 = ORIENTED_EDGE('',*,*,#521,.F.) ;
#655 = ORIENTED_EDGE('',*,*,#522,.T.) ;
#656 = ORIENTED_EDGE('',*,*,#517,.F.) ;
#657 = ORIENTED_EDGE('',*,*,#501,.F.) ;
#658 = ORIENTED_EDGE('',*,*,#504,.F.) ;
#659 = ORIENTED_EDGE('',*,*,#507,.F.) ;
#660 = ORIENTED_EDGE('',*,*,#510,.F.) ;
#661 = ORIENTED_EDGE('',*,*,#513,.F.) ;
#662 = ORIENTED_EDGE('',*,*,#516,.F.) ;
#663 = ORIENTED_EDGE('',*,*,#520,.F.) ;
#664 = ORIENTED_EDGE('',*,*,#519,.T.) ;
#665 = ORIENTED_EDGE('',*,*,#499,.T.) ;
#666 = ORIENTED_EDGE('',*,*,#502,.T.) ;
#667 = ORIENTED_EDGE('',*,*,#505,.T.) ;
#668 = ORIENTED_EDGE('',*,*,#508,.T.) ;
#669 = ORIENTED_EDGE('',*,*,#511,.T.) ;
#670 = ORIENTED_EDGE('',*,*,#514,.T.) ;
#671 = ORIENTED_EDGE('',*,*,#523,.F.) ;
#672 = ORIENTED_EDGE('',*,*,#524,.T.) ;
#673 = ORIENTED_EDGE('',*,*,#525,.F.) ;
#674 = ORIENTED_EDGE('',*,*,#524,.F.) ;
#675 = ORIENTED_EDGE('',*,*,#526,.F.) ;
#676 = ORIENTED_EDGE('',*,*,#527,.T.) ;
#677 = ORIENTED_EDGE('',*,*,#528,.T.) ;
#678 = ORIENTED_EDGE('',*,*,#527,.F.) ;
#679 = ORIENTED_EDGE('',*,*,#529,.F.) ;
#680 = ORIENTED_EDGE('',*,*,#530,.T.) ;
#681 = ORIENTED_EDGE('',*,*,#526,.T.) ;
#682 = ORIENTED_EDGE('',*,*,#530,.F.) ;
#683 = ORIENTED_EDGE('',*,*,#531,.F.) ;
#684 = ORIENTED_EDGE('',*,*,#532,.T.) ;
#685 = ORIENTED_EDGE('',*,*,#529,.T.) ;
#686 = ORIENTED_EDGE('',*,*,#532,.F.) ;
#687 = ORIENTED_EDGE('',*,*,#525,.T.) ;
#688 = ORIENTED_EDGE('',*,*,#533,.T.) ;
#689 = ORIENTED_EDGE('',*,*,#531,.T.) ;
#690 = ORIENTED_EDGE('',*,*,#533,.F.) ;
#691 = ORIENTED_EDGE('',*,*,#534,.F.) ;
#692 = ORIENTED_EDGE('',*,*,#535,.T.) ;
#693 = ORIENTED_EDGE('',*,*,#523,.T.) ;
#694 = ORIENTED_EDGE('',*,*,#535,.F.) ;
#695 = ORIENTED_EDGE('',*,*,#528,.F.) ;
#696 = ORIENTED_EDGE('',*,*,#536,.T.) ;
#697 = ORIENTED_EDGE('',*,*,#534,.T.) ;
#698 = ORIENTED_EDGE('',*,*,#536,.F.) ;
#699 = ORIENTED_EDGE('',*,*,#537,.F.) ;
#700 = ORIENTED_EDGE('',*,*,#538,.T.) ;
#701 = ORIENTED_EDGE('',*,*,#539,.T.) ;
#702 = ORIENTED_EDGE('',*,*,#538,.F.) ;
#703 = ORIENTED_EDGE('',*,*,#540,.F.) ;
#704 = ORIENTED_EDGE('',*,*,#541,.T.) ;
#705 = ORIENTED_EDGE('',*,*,#542,.T.) ;
#706 = ORIENTED_EDGE('',*,*,#541,.F.) ;
#707 = ORIENTED_EDGE('',*,*,#543,.F.) ;
#708 = ORIENTED_EDGE('',*,*,#544,.F.) ;
#709 = ORIENTED_EDGE('',*,*,#545,.T.) ;
#710 = ORIENTED_EDGE('',*,*,#546,.T.) ;
#711 = ORIENTED_EDGE('',*,*,#540,.T.) ;
#712 = ORIENTED_EDGE('',*,*,#547,.T.) ;
#713 = ORIENTED_EDGE('',*,*,#548,.T.) ;
#714 = ORIENTED_EDGE('',*,*,#545,.F.) ;
#715 = ORIENTED_EDGE('',*,*,#549,.T.) ;
#716 = ORIENTED_EDGE('',*,*,#537,.T.) ;
#717 = ORIENTED_EDGE('',*,*,#542,.F.) ;
#718 = ORIENTED_EDGE('',*,*,#539,.F.) ;
#719 = ORIENTED_EDGE('',*,*,#543,.T.) ;
#720 = ORIENTED_EDGE('',*,*,#550,.F.) ;
#721 = ORIENTED_EDGE('',*,*,#551,.F.) ;
#722 = ORIENTED_EDGE('',*,*,#552,.F.) ;
#723 = ORIENTED_EDGE('',*,*,#550,.T.) ;
#724 = ORIENTED_EDGE('',*,*,#546,.F.) ;
#725 = ORIENTED_EDGE('',*,*,#548,.F.) ;
#726 = ORIENTED_EDGE('',*,*,#553,.T.) ;
#727 = ORIENTED_EDGE('',*,*,#551,.T.) ;
#728 = ORIENTED_EDGE('',*,*,#553,.F.) ;
#729 = ORIENTED_EDGE('',*,*,#547,.F.) ;
#730 = ORIENTED_EDGE('',*,*,#554,.T.) ;
#731 = ORIENTED_EDGE('',*,*,#552,.T.) ;
#732 = ORIENTED_EDGE('',*,*,#554,.F.) ;
#733 = ORIENTED_EDGE('',*,*,#549,.F.) ;
#734 = ORIENTED_EDGE('',*,*,#544,.T.) ;
#735 = ORIENTED_EDGE('',*,*,#555,.F.) ;
#736 = ORIENTED_EDGE('',*,*,#556,.F.) ;
#737 = ORIENTED_EDGE('',*,*,#557,.F.) ;
#738 = ORIENTED_EDGE('',*,*,#558,.T.) ;
#739 = ORIENTED_EDGE('',*,*,#559,.F.) ;
#740 = ORIENTED_EDGE('',*,*,#560,.F.) ;
#741 = ORIENTED_EDGE('',*,*,#561,.T.) ;
#742 = ORIENTED_EDGE('',*,*,#562,.T.) ;
#743 = ORIENTED_EDGE('',*,*,#563,.T.) ;
#744 = ORIENTED_EDGE('',*,*,#564,.F.) ;
#745 = ORIENTED_EDGE('',*,*,#565,.F.) ;
#746 = ORIENTED_EDGE('',*,*,#566,.T.) ;
#747 = ORIENTED_EDGE('',*,*,#567,.F.) ;
#748 = ORIENTED_EDGE('',*,*,#568,.F.) ;
#749 = ORIENTED_EDGE('',*,*,#569,.T.) ;
#750 = ORIENTED_EDGE('',*,*,#564,.T.) ;
#751 = ORIENTED_EDGE('',*,*,#570,.F.) ;
#752 = ORIENTED_EDGE('',*,*,#571,.F.) ;
#753 = ORIENTED_EDGE('',*,*,#572,.T.) ;
#754 = ORIENTED_EDGE('',*,*,#568,.T.) ;
#755 = ORIENTED_EDGE('',*,*,#562,.F.) ;
#756 = ORIENTED_EDGE('',*,*,#573,.F.) ;
#757 = ORIENTED_EDGE('',*,*,#556,.T.) ;
#758 = ORIENTED_EDGE('',*,*,#571,.T.) ;
#759 = ORIENTED_EDGE('',*,*,#561,.F.) ;
#760 = ORIENTED_EDGE('',*,*,#574,.F.) ;
#761 = ORIENTED_EDGE('',*,*,#557,.T.) ;
#762 = ORIENTED_EDGE('',*,*,#573,.T.) ;
#763 = ORIENTED_EDGE('',*,*,#560,.T.) ;
#764 = ORIENTED_EDGE('',*,*,#566,.F.) ;
#765 = ORIENTED_EDGE('',*,*,#558,.F.) ;
#766 = ORIENTED_EDGE('',*,*,#574,.T.) ;
#767 = ORIENTED_EDGE('',*,*,#565,.T.) ;
#768 = ORIENTED_EDGE('',*,*,#569,.F.) ;
#769 = ORIENTED_EDGE('',*,*,#572,.F.) ;
#770 = ORIENTED_EDGE('',*,*,#555,.T.) ;
#771 = ORIENTED_EDGE('',*,*,#563,.F.) ;
#772 = ORIENTED_EDGE('',*,*,#559,.T.) ;
#773 = ORIENTED_EDGE('',*,*,#570,.T.) ;
#774 = ORIENTED_EDGE('',*,*,#567,.T.) ;
#775 = CYLINDRICAL_SURFACE('',#907,6.49999999999999) ;
#776 = CYLINDRICAL_SURFACE('',#910,6.49999999999999) ;
#777 = CYLINDRICAL_SURFACE('',#913,6.49999999999999) ;
#778 = CYLINDRICAL_SURFACE('',#916,6.49999999999999) ;
#779 = CYLINDRICAL_SURFACE('',#919,6.49999999999999) ;
#780 = CYLINDRICAL_SURFACE('',#922,6.49999999999999) ;
#781 = CYLINDRICAL_SURFACE('',#925,35.) ;
#782 = CYLINDRICAL_SURFACE('',#928,375.) ;
#783 = CYLINDRICAL_SURFACE('',#934,6.49999999999999) ;
#784 = CYLINDRICAL_SURFACE('',#937,6.49999999999999) ;
#785 = CYLINDRICAL_SURFACE('',#940,6.49999999999999) ;
#786 = CYLINDRICAL_SURFACE('',#943,6.49999999999999) ;
#787 = CYLINDRICAL_SURFACE('',#946,6.49999999999999) ;
#788 = CYLINDRICAL_SURFACE('',#949,6.49999999999999) ;
#789 = CYLINDRICAL_SURFACE('',#952,35.) ;
#790 = CYLINDRICAL_SURFACE('',#955,120.) ;
#791 = CYLINDRICAL_SURFACE('',#968,285.) ;
#792 = CYLINDRICAL_SURFACE('',#973,287.) ;
#793 = CYLINDRICAL_SURFACE('',#979,42.5) ;
#794 = CYLINDRICAL_SURFACE('',#982,35.) ;
#795 = CYLINDRICAL_SURFACE('',#985,19.) ;
#796 = CYLINDRICAL_SURFACE('',#1004,250.) ;
#797 = CYLINDRICAL_SURFACE('',#1006,245.24) ;
#798 = ADVANCED_FACE('',(#141),#775,.F.) ;
#799 = ADVANCED_FACE('',(#142),#776,.F.) ;
#800 = ADVANCED_FACE('',(#143),#777,.F.) ;
#801 = ADVANCED_FACE('',(#144),#778,.F.) ;
#802 = ADVANCED_FACE('',(#145),#779,.F.) ;
#803 = ADVANCED_FACE('',(#146),#780,.F.) ;
#804 = ADVANCED_FACE('',(#147),#781,.F.) ;
#805 = ADVANCED_FACE('',(#148),#782,.T.) ;
#806 = ADVANCED_FACE('',(#149,#92,#93,#94,#95,#96,#97,#98),#123,.F.) ;
#807 = ADVANCED_FACE('',(#150,#99,#100,#101,#102,#103,#104,#105),#124,.T.) ;
#808 = ADVANCED_FACE('',(#151),#783,.F.) ;
#809 = ADVANCED_FACE('',(#152),#784,.F.) ;
#810 = ADVANCED_FACE('',(#153),#785,.F.) ;
#811 = ADVANCED_FACE('',(#154),#786,.F.) ;
#812 = ADVANCED_FACE('',(#155),#787,.F.) ;
#813 = ADVANCED_FACE('',(#156),#788,.F.) ;
#814 = ADVANCED_FACE('',(#157),#789,.F.) ;
#815 = ADVANCED_FACE('',(#158),#790,.T.) ;
#816 = ADVANCED_FACE('',(#159,#106,#107,#108,#109,#110,#111,#112),#125,.T.) ;
#817 = ADVANCED_FACE('',(#160,#113,#114,#115,#116,#117,#118,#119),#126,.F.) ;
#818 = ADVANCED_FACE('',(#161),#69,.F.) ;
#819 = ADVANCED_FACE('',(#162),#67,.F.) ;
#820 = ADVANCED_FACE('',(#163),#791,.F.) ;
#821 = ADVANCED_FACE('',(#164),#70,.T.) ;
#822 = ADVANCED_FACE('',(#165),#792,.T.) ;
#823 = ADVANCED_FACE('',(#166),#68,.T.) ;
#824 = ADVANCED_FACE('',(#167),#71,.T.) ;
#825 = ADVANCED_FACE('',(#168),#793,.T.) ;
#826 = ADVANCED_FACE('',(#169),#794,.T.) ;
#827 = ADVANCED_FACE('',(#170),#795,.F.) ;
#828 = ADVANCED_FACE('',(#171,#120),#127,.F.) ;
#829 = ADVANCED_FACE('',(#172,#121),#128,.F.) ;
#830 = ADVANCED_FACE('',(#173,#122),#129,.F.) ;
#831 = ADVANCED_FACE('',(#174),#130,.F.) ;
#832 = ADVANCED_FACE('',(#175),#131,.F.) ;
#833 = ADVANCED_FACE('',(#176),#132,.F.) ;
#834 = ADVANCED_FACE('',(#177),#133,.T.) ;
#835 = ADVANCED_FACE('',(#178),#134,.T.) ;
#836 = ADVANCED_FACE('',(#179),#135,.F.) ;
#837 = ADVANCED_FACE('',(#180),#136,.T.) ;
#838 = ADVANCED_FACE('',(#181),#137,.T.) ;
#839 = ADVANCED_FACE('',(#182),#796,.T.) ;
#840 = ADVANCED_FACE('',(#183),#138,.T.) ;
#841 = ADVANCED_FACE('',(#184),#797,.F.) ;
#842 = ADVANCED_FACE('',(#185),#139,.F.) ;
#843 = ADVANCED_FACE('',(#186),#140,.T.) ;
#844 = CLOSED_SHELL('',(#798,#799,#800,#801,#802,#803,#804,#805,#806,#807)) ;
#845 = CLOSED_SHELL('',(#808,#809,#810,#811,#812,#813,#814,#815,#816,#817)) ;
#846 = CLOSED_SHELL('',(#818,#819,#820,#821,#822,#823,#824)) ;
#847 = CLOSED_SHELL('',(#825,#826,#827,#828,#829,#830,#831,#832,#833)) ;
#848 = CLOSED_SHELL('',(#834,#835,#836,#837,#838,#839,#840,#841,#842,#843)) ;
#849 = DERIVED_UNIT_ELEMENT(#859,1.) ;
#850 = DERIVED_UNIT_ELEMENT(#1551,-3.) ;
#851 = DERIVED_UNIT_ELEMENT(#859,1.) ;
#852 = DERIVED_UNIT_ELEMENT(#1551,-3.) ;
#853 = DERIVED_UNIT_ELEMENT(#859,1.) ;
#854 = DERIVED_UNIT_ELEMENT(#1551,-3.) ;
#855 = DERIVED_UNIT_ELEMENT(#859,1.) ;
#856 = DERIVED_UNIT_ELEMENT(#1551,-3.) ;
#857 = DERIVED_UNIT_ELEMENT(#859,1.) ;
#858 = DERIVED_UNIT_ELEMENT(#1551,-3.) ;
#859 = (
MASS_UNIT()
NAMED_UNIT(*)
SI_UNIT(.KILO.,.GRAM.)
) ;
#860 = DERIVED_UNIT((#849,#850)) ;
#861 = DERIVED_UNIT((#851,#852)) ;
#862 = DERIVED_UNIT((#853,#854)) ;
#863 = DERIVED_UNIT((#855,#856)) ;
#864 = DERIVED_UNIT((#857,#858)) ;
#865 = MEASURE_REPRESENTATION_ITEM('density measure',
POSITIVE_RATIO_MEASURE(7850.),#860) ;
#866 = MEASURE_REPRESENTATION_ITEM('density measure',
POSITIVE_RATIO_MEASURE(7850.),#861) ;
#867 = MEASURE_REPRESENTATION_ITEM('density measure',
POSITIVE_RATIO_MEASURE(7850.),#862) ;
#868 = MEASURE_REPRESENTATION_ITEM('density measure',
POSITIVE_RATIO_MEASURE(7850.),#863) ;
#869 = MEASURE_REPRESENTATION_ITEM('density measure',
POSITIVE_RATIO_MEASURE(7850.),#864) ;
#870 = PROPERTY_DEFINITION_REPRESENTATION(#895,#880) ;
#871 = PROPERTY_DEFINITION_REPRESENTATION(#896,#881) ;
#872 = PROPERTY_DEFINITION_REPRESENTATION(#897,#882) ;
#873 = PROPERTY_DEFINITION_REPRESENTATION(#898,#883) ;
#874 = PROPERTY_DEFINITION_REPRESENTATION(#899,#884) ;
#875 = PROPERTY_DEFINITION_REPRESENTATION(#900,#885) ;
#876 = PROPERTY_DEFINITION_REPRESENTATION(#901,#886) ;
#877 = PROPERTY_DEFINITION_REPRESENTATION(#902,#887) ;
#878 = PROPERTY_DEFINITION_REPRESENTATION(#903,#888) ;
#879 = PROPERTY_DEFINITION_REPRESENTATION(#904,#889) ;
#880 = REPRESENTATION('material name',(#890),#1544) ;
#881 = REPRESENTATION('density',(#865),#1544) ;
#882 = REPRESENTATION('material name',(#891),#1545) ;
#883 = REPRESENTATION('density',(#866),#1545) ;
#884 = REPRESENTATION('material name',(#892),#1546) ;
#885 = REPRESENTATION('density',(#867),#1546) ;
#886 = REPRESENTATION('material name',(#893),#1547) ;
#887 = REPRESENTATION('density',(#868),#1547) ;
#888 = REPRESENTATION('material name',(#894),#1548) ;
#889 = REPRESENTATION('density',(#869),#1548) ;
#890 = DESCRIPTIVE_REPRESENTATION_ITEM('Steel','Steel') ;
#891 = DESCRIPTIVE_REPRESENTATION_ITEM('Steel','Steel') ;
#892 = DESCRIPTIVE_REPRESENTATION_ITEM('Steel','Steel') ;
#893 = DESCRIPTIVE_REPRESENTATION_ITEM('Steel','Steel') ;
#894 = DESCRIPTIVE_REPRESENTATION_ITEM('Steel','Steel') ;
#895 = PROPERTY_DEFINITION('material property','material name',#1588) ;
#896 = PROPERTY_DEFINITION('material property','density of part',#1588) ;
#897 = PROPERTY_DEFINITION('material property','material name',#1589) ;
#898 = PROPERTY_DEFINITION('material property','density of part',#1589) ;
#899 = PROPERTY_DEFINITION('material property','material name',#1590) ;
#900 = PROPERTY_DEFINITION('material property','density of part',#1590) ;
#901 = PROPERTY_DEFINITION('material property','material name',#1591) ;
#902 = PROPERTY_DEFINITION('material property','density of part',#1591) ;
#903 = PROPERTY_DEFINITION('material property','material name',#1592) ;
#904 = PROPERTY_DEFINITION('material property','density of part',#1592) ;
#905 = AXIS2_PLACEMENT_3D('',#1307,#1023,#1024) ;
#906 = AXIS2_PLACEMENT_3D('',#1308,#1025,#1026) ;
#907 = AXIS2_PLACEMENT_3D('',#1309,#1027,#1028) ;
#908 = AXIS2_PLACEMENT_3D('',#1311,#1029,#1030) ;
#909 = AXIS2_PLACEMENT_3D('',#1314,#1032,#1033) ;
#910 = AXIS2_PLACEMENT_3D('',#1315,#1034,#1035) ;
#911 = AXIS2_PLACEMENT_3D('',#1317,#1036,#1037) ;
#912 = AXIS2_PLACEMENT_3D('',#1320,#1039,#1040) ;
#913 = AXIS2_PLACEMENT_3D('',#1321,#1041,#1042) ;
#914 = AXIS2_PLACEMENT_3D('',#1323,#1043,#1044) ;
#915 = AXIS2_PLACEMENT_3D('',#1326,#1046,#1047) ;
#916 = AXIS2_PLACEMENT_3D('',#1327,#1048,#1049) ;
#917 = AXIS2_PLACEMENT_3D('',#1329,#1050,#1051) ;
#918 = AXIS2_PLACEMENT_3D('',#1332,#1053,#1054) ;
#919 = AXIS2_PLACEMENT_3D('',#1333,#1055,#1056) ;
#920 = AXIS2_PLACEMENT_3D('',#1335,#1057,#1058) ;
#921 = AXIS2_PLACEMENT_3D('',#1338,#1060,#1061) ;
#922 = AXIS2_PLACEMENT_3D('',#1339,#1062,#1063) ;
#923 = AXIS2_PLACEMENT_3D('',#1341,#1064,#1065) ;
#924 = AXIS2_PLACEMENT_3D('',#1344,#1067,#1068) ;
#925 = AXIS2_PLACEMENT_3D('',#1345,#1069,#1070) ;
#926 = AXIS2_PLACEMENT_3D('',#1347,#1071,#1072) ;
#927 = AXIS2_PLACEMENT_3D('',#1350,#1074,#1075) ;
#928 = AXIS2_PLACEMENT_3D('',#1351,#1076,#1077) ;
#929 = AXIS2_PLACEMENT_3D('',#1353,#1078,#1079) ;
#930 = AXIS2_PLACEMENT_3D('',#1356,#1081,#1082) ;
#931 = AXIS2_PLACEMENT_3D('',#1357,#1083,#1084) ;
#932 = AXIS2_PLACEMENT_3D('',#1358,#1085,#1086) ;
#933 = AXIS2_PLACEMENT_3D('',#1359,#1087,#1088) ;
#934 = AXIS2_PLACEMENT_3D('',#1360,#1089,#1090) ;
#935 = AXIS2_PLACEMENT_3D('',#1362,#1091,#1092) ;
#936 = AXIS2_PLACEMENT_3D('',#1365,#1094,#1095) ;
#937 = AXIS2_PLACEMENT_3D('',#1366,#1096,#1097) ;
#938 = AXIS2_PLACEMENT_3D('',#1368,#1098,#1099) ;
#939 = AXIS2_PLACEMENT_3D('',#1371,#1101,#1102) ;
#940 = AXIS2_PLACEMENT_3D('',#1372,#1103,#1104) ;
#941 = AXIS2_PLACEMENT_3D('',#1374,#1105,#1106) ;
#942 = AXIS2_PLACEMENT_3D('',#1377,#1108,#1109) ;
#943 = AXIS2_PLACEMENT_3D('',#1378,#1110,#1111) ;
#944 = AXIS2_PLACEMENT_3D('',#1380,#1112,#1113) ;
#945 = AXIS2_PLACEMENT_3D('',#1383,#1115,#1116) ;
#946 = AXIS2_PLACEMENT_3D('',#1384,#1117,#1118) ;
#947 = AXIS2_PLACEMENT_3D('',#1386,#1119,#1120) ;
#948 = AXIS2_PLACEMENT_3D('',#1389,#1122,#1123) ;
#949 = AXIS2_PLACEMENT_3D('',#1390,#1124,#1125) ;
#950 = AXIS2_PLACEMENT_3D('',#1392,#1126,#1127) ;
#951 = AXIS2_PLACEMENT_3D('',#1395,#1129,#1130) ;
#952 = AXIS2_PLACEMENT_3D('',#1396,#1131,#1132) ;
#953 = AXIS2_PLACEMENT_3D('',#1398,#1133,#1134) ;
#954 = AXIS2_PLACEMENT_3D('',#1401,#1136,#1137) ;
#955 = AXIS2_PLACEMENT_3D('',#1402,#1138,#1139) ;
#956 = AXIS2_PLACEMENT_3D('',#1404,#1140,#1141) ;
#957 = AXIS2_PLACEMENT_3D('',#1407,#1143,#1144) ;
#958 = AXIS2_PLACEMENT_3D('',#1408,#1145,#1146) ;
#959 = AXIS2_PLACEMENT_3D('',#1409,#1147,#1148) ;
#960 = AXIS2_PLACEMENT_3D('',#1410,#1149,#1150) ;
#961 = AXIS2_PLACEMENT_3D('',#1411,#1151,#1152) ;
#962 = AXIS2_PLACEMENT_3D('',#1413,#1153,#1154) ;
#963 = AXIS2_PLACEMENT_3D('',#1415,#1155,#1156) ;
#964 = AXIS2_PLACEMENT_3D('',#1416,#1157,#1158) ;
#965 = AXIS2_PLACEMENT_3D('',#1417,#1159,#1160) ;
#966 = AXIS2_PLACEMENT_3D('',#1419,#1161,#1162) ;
#967 = AXIS2_PLACEMENT_3D('',#1422,#1164,#1165) ;
#968 = AXIS2_PLACEMENT_3D('',#1423,#1166,#1167) ;
#969 = AXIS2_PLACEMENT_3D('',#1425,#1168,#1169) ;
#970 = AXIS2_PLACEMENT_3D('',#1427,#1171,#1172) ;
#971 = AXIS2_PLACEMENT_3D('',#1429,#1173,#1174) ;
#972 = AXIS2_PLACEMENT_3D('',#1430,#1175,#1176) ;
#973 = AXIS2_PLACEMENT_3D('',#1431,#1177,#1178) ;
#974 = AXIS2_PLACEMENT_3D('',#1433,#1180,#1181) ;
#975 = AXIS2_PLACEMENT_3D('',#1435,#1182,#1183) ;
#976 = AXIS2_PLACEMENT_3D('',#1437,#1185,#1186) ;
#977 = AXIS2_PLACEMENT_3D('',#1438,#1187,#1188) ;
#978 = AXIS2_PLACEMENT_3D('',#1439,#1189,#1190) ;
#979 = AXIS2_PLACEMENT_3D('',#1440,#1191,#1192) ;
#980 = AXIS2_PLACEMENT_3D('',#1442,#1193,#1194) ;
#981 = AXIS2_PLACEMENT_3D('',#1445,#1196,#1197) ;
#982 = AXIS2_PLACEMENT_3D('',#1446,#1198,#1199) ;
#983 = AXIS2_PLACEMENT_3D('',#1448,#1200,#1201) ;
#984 = AXIS2_PLACEMENT_3D('',#1451,#1203,#1204) ;
#985 = AXIS2_PLACEMENT_3D('',#1452,#1205,#1206) ;
#986 = AXIS2_PLACEMENT_3D('',#1455,#1207,#1208) ;
#987 = AXIS2_PLACEMENT_3D('',#1459,#1210,#1211) ;
#988 = AXIS2_PLACEMENT_3D('',#1461,#1213,#1214) ;
#989 = AXIS2_PLACEMENT_3D('',#1467,#1218,#1219) ;
#990 = AXIS2_PLACEMENT_3D('',#1468,#1220,#1221) ;
#991 = AXIS2_PLACEMENT_3D('',#1474,#1225,#1226) ;
#992 = AXIS2_PLACEMENT_3D('',#1476,#1228,#1229) ;
#993 = AXIS2_PLACEMENT_3D('',#1478,#1231,#1232) ;
#994 = AXIS2_PLACEMENT_3D('',#1479,#1233,#1234) ;
#995 = AXIS2_PLACEMENT_3D('',#1480,#1235,#1236) ;
#996 = AXIS2_PLACEMENT_3D('',#1485,#1238,#1239) ;
#997 = AXIS2_PLACEMENT_3D('',#1488,#1241,#1242) ;
#998 = AXIS2_PLACEMENT_3D('',#1489,#1243,#1244) ;
#999 = AXIS2_PLACEMENT_3D('',#1494,#1246,#1247) ;
#1000 = AXIS2_PLACEMENT_3D('',#1497,#1249,#1250) ;
#1001 = AXIS2_PLACEMENT_3D('',#1498,#1251,#1252) ;
#1002 = AXIS2_PLACEMENT_3D('',#1505,#1257,#1258) ;
#1003 = AXIS2_PLACEMENT_3D('',#1511,#1262,#1263) ;
#1004 = AXIS2_PLACEMENT_3D('',#1515,#1267,#1268) ;
#1005 = AXIS2_PLACEMENT_3D('',#1517,#1270,#1271) ;
#1006 = AXIS2_PLACEMENT_3D('',#1519,#1273,#1274) ;
#1007 = AXIS2_PLACEMENT_3D('',#1520,#1275,#1276) ;
#1008 = AXIS2_PLACEMENT_3D('',#1521,#1277,#1278) ;
#1009 = AXIS2_PLACEMENT_3D('',#1522,#1279,#1280) ;
#1010 = AXIS2_PLACEMENT_3D('',#1523,#1281,#1282) ;
#1011 = AXIS2_PLACEMENT_3D('',#1524,#1283,#1284) ;
#1012 = AXIS2_PLACEMENT_3D('',#1525,#1285,#1286) ;
#1013 = AXIS2_PLACEMENT_3D('',#1526,#1287,#1288) ;
#1014 = AXIS2_PLACEMENT_3D('',#1527,#1289,#1290) ;
#1015 = AXIS2_PLACEMENT_3D('',#1528,#1291,#1292) ;
#1016 = AXIS2_PLACEMENT_3D('',#1529,#1293,#1294) ;
#1017 = AXIS2_PLACEMENT_3D('',#1530,#1295,#1296) ;
#1018 = AXIS2_PLACEMENT_3D('',#1531,#1297,#1298) ;
#1019 = AXIS2_PLACEMENT_3D('',#1532,#1299,#1300) ;
#1020 = AXIS2_PLACEMENT_3D('',#1533,#1301,#1302) ;
#1021 = AXIS2_PLACEMENT_3D('',#1534,#1303,#1304) ;
#1022 = AXIS2_PLACEMENT_3D('',#1535,#1305,#1306) ;
#1023 = DIRECTION('axis',(0.,0.,1.)) ;
#1024 = DIRECTION('refdir',(1.,0.,0.)) ;
#1025 = DIRECTION('axis',(0.,0.,1.)) ;
#1026 = DIRECTION('refdir',(1.,0.,0.)) ;
#1027 = DIRECTION('center_axis',(1.,0.,0.)) ;
#1028 = DIRECTION('ref_axis',(0.,0.,-1.)) ;
#1029 = DIRECTION('center_axis',(1.,0.,0.)) ;
#1030 = DIRECTION('ref_axis',(0.,0.,-1.)) ;
#1031 = DIRECTION('',(1.,0.,0.)) ;
#1032 = DIRECTION('center_axis',(1.,0.,0.)) ;
#1033 = DIRECTION('ref_axis',(0.,0.,-1.)) ;
#1034 = DIRECTION('center_axis',(1.,0.,0.)) ;
#1035 = DIRECTION('ref_axis',(0.,0.,-1.)) ;
#1036 = DIRECTION('center_axis',(1.,0.,0.)) ;
#1037 = DIRECTION('ref_axis',(0.,0.,-1.)) ;
#1038 = DIRECTION('',(1.,0.,0.)) ;
#1039 = DIRECTION('center_axis',(1.,0.,0.)) ;
#1040 = DIRECTION('ref_axis',(0.,0.,-1.)) ;
#1041 = DIRECTION('center_axis',(1.,0.,0.)) ;
#1042 = DIRECTION('ref_axis',(0.,0.,-1.)) ;
#1043 = DIRECTION('center_axis',(1.,0.,0.)) ;
#1044 = DIRECTION('ref_axis',(0.,0.,-1.)) ;
#1045 = DIRECTION('',(1.,0.,0.)) ;
#1046 = DIRECTION('center_axis',(1.,0.,0.)) ;
#1047 = DIRECTION('ref_axis',(0.,0.,-1.)) ;
#1048 = DIRECTION('center_axis',(1.,0.,0.)) ;
#1049 = DIRECTION('ref_axis',(0.,0.,-1.)) ;
#1050 = DIRECTION('center_axis',(1.,0.,0.)) ;
#1051 = DIRECTION('ref_axis',(0.,0.,-1.)) ;
#1052 = DIRECTION('',(1.,0.,0.)) ;
#1053 = DIRECTION('center_axis',(1.,0.,0.)) ;
#1054 = DIRECTION('ref_axis',(0.,0.,-1.)) ;
#1055 = DIRECTION('center_axis',(1.,0.,0.)) ;
#1056 = DIRECTION('ref_axis',(0.,0.,-1.)) ;
#1057 = DIRECTION('center_axis',(1.,0.,0.)) ;
#1058 = DIRECTION('ref_axis',(0.,0.,-1.)) ;
#1059 = DIRECTION('',(1.,0.,0.)) ;
#1060 = DIRECTION('center_axis',(1.,0.,0.)) ;
#1061 = DIRECTION('ref_axis',(0.,0.,-1.)) ;
#1062 = DIRECTION('center_axis',(1.,0.,0.)) ;
#1063 = DIRECTION('ref_axis',(0.,0.,-1.)) ;
#1064 = DIRECTION('center_axis',(1.,0.,0.)) ;
#1065 = DIRECTION('ref_axis',(0.,0.,-1.)) ;
#1066 = DIRECTION('',(1.,0.,0.)) ;
#1067 = DIRECTION('center_axis',(1.,0.,0.)) ;
#1068 = DIRECTION('ref_axis',(0.,0.,-1.)) ;
#1069 = DIRECTION('center_axis',(1.,0.,0.)) ;
#1070 = DIRECTION('ref_axis',(0.,0.,-1.)) ;
#1071 = DIRECTION('center_axis',(1.,0.,0.)) ;
#1072 = DIRECTION('ref_axis',(0.,0.,-1.)) ;
#1073 = DIRECTION('',(1.,0.,0.)) ;
#1074 = DIRECTION('center_axis',(1.,0.,0.)) ;
#1075 = DIRECTION('ref_axis',(0.,0.,-1.)) ;
#1076 = DIRECTION('center_axis',(1.,0.,0.)) ;
#1077 = DIRECTION('ref_axis',(0.,0.,-1.)) ;
#1078 = DIRECTION('center_axis',(1.,0.,0.)) ;
#1079 = DIRECTION('ref_axis',(0.,0.,-1.)) ;
#1080 = DIRECTION('',(-1.,0.,0.)) ;
#1081 = DIRECTION('center_axis',(1.,0.,0.)) ;
#1082 = DIRECTION('ref_axis',(0.,0.,-1.)) ;
#1083 = DIRECTION('center_axis',(1.,0.,0.)) ;
#1084 = DIRECTION('ref_axis',(0.,0.,-1.)) ;
#1085 = DIRECTION('center_axis',(1.,0.,0.)) ;
#1086 = DIRECTION('ref_axis',(0.,0.,-1.)) ;
#1087 = DIRECTION('axis',(0.,0.,1.)) ;
#1088 = DIRECTION('refdir',(1.,0.,0.)) ;
#1089 = DIRECTION('center_axis',(1.,0.,0.)) ;
#1090 = DIRECTION('ref_axis',(0.,0.,-1.)) ;
#1091 = DIRECTION('center_axis',(1.,0.,0.)) ;
#1092 = DIRECTION('ref_axis',(0.,0.,-1.)) ;
#1093 = DIRECTION('',(1.,0.,0.)) ;
#1094 = DIRECTION('center_axis',(1.,0.,0.)) ;
#1095 = DIRECTION('ref_axis',(0.,0.,-1.)) ;
#1096 = DIRECTION('center_axis',(1.,0.,0.)) ;
#1097 = DIRECTION('ref_axis',(0.,0.,-1.)) ;
#1098 = DIRECTION('center_axis',(1.,0.,0.)) ;
#1099 = DIRECTION('ref_axis',(0.,0.,-1.)) ;
#1100 = DIRECTION('',(1.,0.,0.)) ;
#1101 = DIRECTION('center_axis',(1.,0.,0.)) ;
#1102 = DIRECTION('ref_axis',(0.,0.,-1.)) ;
#1103 = DIRECTION('center_axis',(1.,0.,0.)) ;
#1104 = DIRECTION('ref_axis',(0.,0.,-1.)) ;
#1105 = DIRECTION('center_axis',(1.,0.,0.)) ;
#1106 = DIRECTION('ref_axis',(0.,0.,-1.)) ;
#1107 = DIRECTION('',(1.,0.,0.)) ;
#1108 = DIRECTION('center_axis',(1.,0.,0.)) ;
#1109 = DIRECTION('ref_axis',(0.,0.,-1.)) ;
#1110 = DIRECTION('center_axis',(1.,0.,0.)) ;
#1111 = DIRECTION('ref_axis',(0.,0.,-1.)) ;
#1112 = DIRECTION('center_axis',(1.,0.,0.)) ;
#1113 = DIRECTION('ref_axis',(0.,0.,-1.)) ;
#1114 = DIRECTION('',(1.,0.,0.)) ;
#1115 = DIRECTION('center_axis',(1.,0.,0.)) ;
#1116 = DIRECTION('ref_axis',(0.,0.,-1.)) ;
#1117 = DIRECTION('center_axis',(1.,0.,0.)) ;
#1118 = DIRECTION('ref_axis',(0.,0.,-1.)) ;
#1119 = DIRECTION('center_axis',(1.,0.,0.)) ;
#1120 = DIRECTION('ref_axis',(0.,0.,-1.)) ;
#1121 = DIRECTION('',(1.,0.,0.)) ;
#1122 = DIRECTION('center_axis',(1.,0.,0.)) ;
#1123 = DIRECTION('ref_axis',(0.,0.,-1.)) ;
#1124 = DIRECTION('center_axis',(1.,0.,0.)) ;
#1125 = DIRECTION('ref_axis',(0.,0.,-1.)) ;
#1126 = DIRECTION('center_axis',(1.,0.,0.)) ;
#1127 = DIRECTION('ref_axis',(0.,0.,-1.)) ;
#1128 = DIRECTION('',(1.,0.,0.)) ;
#1129 = DIRECTION('center_axis',(1.,0.,0.)) ;
#1130 = DIRECTION('ref_axis',(0.,0.,-1.)) ;
#1131 = DIRECTION('center_axis',(-1.,0.,0.)) ;
#1132 = DIRECTION('ref_axis',(0.,0.,1.)) ;
#1133 = DIRECTION('center_axis',(1.,0.,0.)) ;
#1134 = DIRECTION('ref_axis',(0.,0.,-1.)) ;
#1135 = DIRECTION('',(-1.,0.,0.)) ;
#1136 = DIRECTION('center_axis',(1.,0.,0.)) ;
#1137 = DIRECTION('ref_axis',(0.,0.,-1.)) ;
#1138 = DIRECTION('center_axis',(-1.,0.,0.)) ;
#1139 = DIRECTION('ref_axis',(0.,0.,1.)) ;
#1140 = DIRECTION('center_axis',(1.,0.,0.)) ;
#1141 = DIRECTION('ref_axis',(0.,0.,-1.)) ;
#1142 = DIRECTION('',(1.,0.,0.)) ;
#1143 = DIRECTION('center_axis',(1.,0.,0.)) ;
#1144 = DIRECTION('ref_axis',(0.,0.,-1.)) ;
#1145 = DIRECTION('center_axis',(1.,0.,0.)) ;
#1146 = DIRECTION('ref_axis',(0.,0.,-1.)) ;
#1147 = DIRECTION('center_axis',(1.,0.,0.)) ;
#1148 = DIRECTION('ref_axis',(0.,0.,-1.)) ;
#1149 = DIRECTION('axis',(0.,0.,1.)) ;
#1150 = DIRECTION('refdir',(1.,0.,0.)) ;
#1151 = DIRECTION('center_axis',(0.,-1.,0.)) ;
#1152 = DIRECTION('ref_axis',(0.,0.,-1.)) ;
#1153 = DIRECTION('center_axis',(0.,-1.,0.)) ;
#1154 = DIRECTION('ref_axis',(0.,0.,-1.)) ;
#1155 = DIRECTION('center_axis',(1.,0.,1.22464679914735E-16)) ;
#1156 = DIRECTION('ref_axis',(-1.22464679914735E-16,0.,1.)) ;
#1157 = DIRECTION('center_axis',(0.,1.,0.)) ;
#1158 = DIRECTION('ref_axis',(0.,0.,-1.)) ;
#1159 = DIRECTION('center_axis',(0.,-1.,0.)) ;
#1160 = DIRECTION('ref_axis',(0.,0.,-1.)) ;
#1161 = DIRECTION('center_axis',(0.,-1.,0.)) ;
#1162 = DIRECTION('ref_axis',(0.,0.,-1.)) ;
#1163 = DIRECTION('',(-7.43346104024374E-17,-0.794710876250949,0.606988157354366)) ;
#1164 = DIRECTION('center_axis',(0.,-1.,0.)) ;
#1165 = DIRECTION('ref_axis',(0.,0.,-1.)) ;
#1166 = DIRECTION('center_axis',(0.,-1.,0.)) ;
#1167 = DIRECTION('ref_axis',(0.,0.,-1.)) ;
#1168 = DIRECTION('center_axis',(0.,-1.,0.)) ;
#1169 = DIRECTION('ref_axis',(0.,0.,-1.)) ;
#1170 = DIRECTION('',(0.,-1.,0.)) ;
#1171 = DIRECTION('center_axis',(0.,-1.,0.)) ;
#1172 = DIRECTION('ref_axis',(0.,0.,-1.)) ;
#1173 = DIRECTION('center_axis',(0.,-1.,0.)) ;
#1174 = DIRECTION('ref_axis',(0.,0.,-1.)) ;
#1175 = DIRECTION('center_axis',(-1.,0.,-1.22464679914735E-16)) ;
#1176 = DIRECTION('ref_axis',(-1.22464679914735E-16,0.,1.)) ;
#1177 = DIRECTION('center_axis',(0.,-1.,0.)) ;
#1178 = DIRECTION('ref_axis',(0.,0.,-1.)) ;
#1179 = DIRECTION('',(0.,1.,0.)) ;
#1180 = DIRECTION('center_axis',(0.,-1.,0.)) ;
#1181 = DIRECTION('ref_axis',(0.,0.,-1.)) ;
#1182 = DIRECTION('center_axis',(0.,-1.,0.)) ;
#1183 = DIRECTION('ref_axis',(0.,0.,-1.)) ;
#1184 = DIRECTION('',(7.43346104024374E-17,0.794710876250949,-0.606988157354366)) ;
#1185 = DIRECTION('center_axis',(0.,-1.,0.)) ;
#1186 = DIRECTION('ref_axis',(0.,0.,-1.)) ;
#1187 = DIRECTION('center_axis',(-1.,0.,-1.22464679914735E-16)) ;
#1188 = DIRECTION('ref_axis',(-1.22464679914735E-16,0.,1.)) ;
#1189 = DIRECTION('axis',(0.,0.,1.)) ;
#1190 = DIRECTION('refdir',(1.,0.,0.)) ;
#1191 = DIRECTION('center_axis',(-1.,0.,0.)) ;
#1192 = DIRECTION('ref_axis',(0.,0.,1.)) ;
#1193 = DIRECTION('center_axis',(-1.,0.,0.)) ;
#1194 = DIRECTION('ref_axis',(0.,0.,1.)) ;
#1195 = DIRECTION('',(1.,0.,0.)) ;
#1196 = DIRECTION('center_axis',(-1.,0.,0.)) ;
#1197 = DIRECTION('ref_axis',(0.,0.,1.)) ;
#1198 = DIRECTION('center_axis',(-1.,0.,0.)) ;
#1199 = DIRECTION('ref_axis',(0.,0.,1.)) ;
#1200 = DIRECTION('center_axis',(-1.,0.,0.)) ;
#1201 = DIRECTION('ref_axis',(0.,0.,1.)) ;
#1202 = DIRECTION('',(1.,0.,0.)) ;
#1203 = DIRECTION('center_axis',(-1.,0.,0.)) ;
#1204 = DIRECTION('ref_axis',(0.,0.,1.)) ;
#1205 = DIRECTION('center_axis',(-1.,0.,0.)) ;
#1206 = DIRECTION('ref_axis',(0.,-1.,-1.83697019872103E-16)) ;
#1207 = DIRECTION('center_axis',(-1.,0.,0.)) ;
#1208 = DIRECTION('ref_axis',(0.,0.,1.)) ;
#1209 = DIRECTION('',(1.,0.,0.)) ;
#1210 = DIRECTION('center_axis',(-1.,0.,0.)) ;
#1211 = DIRECTION('ref_axis',(0.,0.,1.)) ;
#1212 = DIRECTION('',(1.,0.,0.)) ;
#1213 = DIRECTION('center_axis',(1.,0.,0.)) ;
#1214 = DIRECTION('ref_axis',(0.,0.,-1.)) ;
#1215 = DIRECTION('',(0.,0.,1.)) ;
#1216 = DIRECTION('',(0.,-1.,0.)) ;
#1217 = DIRECTION('',(0.,1.,2.18495691202819E-16)) ;
#1218 = DIRECTION('center_axis',(1.,0.,0.)) ;
#1219 = DIRECTION('ref_axis',(0.,0.,-1.)) ;
#1220 = DIRECTION('center_axis',(-1.,0.,0.)) ;
#1221 = DIRECTION('ref_axis',(0.,0.,1.)) ;
#1222 = DIRECTION('',(0.,-1.,0.)) ;
#1223 = DIRECTION('',(0.,0.,1.)) ;
#1224 = DIRECTION('',(0.,1.,2.18495691202819E-16)) ;
#1225 = DIRECTION('center_axis',(0.,0.,1.)) ;
#1226 = DIRECTION('ref_axis',(1.,0.,0.)) ;
#1227 = DIRECTION('',(1.,0.,0.)) ;
#1228 = DIRECTION('center_axis',(0.,1.,0.)) ;
#1229 = DIRECTION('ref_axis',(0.,0.,1.)) ;
#1230 = DIRECTION('',(1.,0.,0.)) ;
#1231 = DIRECTION('center_axis',(0.,2.18495691202819E-16,-1.)) ;
#1232 = DIRECTION('ref_axis',(0.,1.,2.18495691202819E-16)) ;
#1233 = DIRECTION('axis',(0.,0.,1.)) ;
#1234 = DIRECTION('refdir',(1.,0.,0.)) ;
#1235 = DIRECTION('center_axis',(1.,0.,0.)) ;
#1236 = DIRECTION('ref_axis',(0.,0.,-1.)) ;
#1237 = DIRECTION('',(0.,-1.,0.)) ;
#1238 = DIRECTION('center_axis',(-1.,0.,0.)) ;
#1239 = DIRECTION('ref_axis',(0.,0.,1.)) ;
#1240 = DIRECTION('',(0.,0.70710678118655,0.707106781186545)) ;
#1241 = DIRECTION('center_axis',(-1.,0.,0.)) ;
#1242 = DIRECTION('ref_axis',(0.,1.77635683940025E-15,-1.)) ;
#1243 = DIRECTION('center_axis',(-1.,0.,0.)) ;
#1244 = DIRECTION('ref_axis',(0.,0.,1.)) ;
#1245 = DIRECTION('',(0.,1.,0.)) ;
#1246 = DIRECTION('center_axis',(-1.,0.,0.)) ;
#1247 = DIRECTION('ref_axis',(0.,1.77635683940025E-15,-1.)) ;
#1248 = DIRECTION('',(0.,0.70710678118655,0.707106781186545)) ;
#1249 = DIRECTION('center_axis',(-1.,0.,0.)) ;
#1250 = DIRECTION('ref_axis',(0.,0.,1.)) ;
#1251 = DIRECTION('center_axis',(0.,1.,0.)) ;
#1252 = DIRECTION('ref_axis',(0.,0.,1.)) ;
#1253 = DIRECTION('',(0.,0.,-1.)) ;
#1254 = DIRECTION('',(-1.,0.,0.)) ;
#1255 = DIRECTION('',(0.,0.,-1.)) ;
#1256 = DIRECTION('',(-1.,0.,0.)) ;
#1257 = DIRECTION('center_axis',(0.,0.,-1.)) ;
#1258 = DIRECTION('ref_axis',(-1.,0.,0.)) ;
#1259 = DIRECTION('',(0.,-1.,0.)) ;
#1260 = DIRECTION('',(-1.,0.,0.)) ;
#1261 = DIRECTION('',(0.,-1.,0.)) ;
#1262 = DIRECTION('center_axis',(0.,1.,0.)) ;
#1263 = DIRECTION('ref_axis',(0.,0.,1.)) ;
#1264 = DIRECTION('',(0.,0.,-1.)) ;
#1265 = DIRECTION('',(-1.,0.,0.)) ;
#1266 = DIRECTION('',(0.,0.,-1.)) ;
#1267 = DIRECTION('center_axis',(-1.,0.,0.)) ;
#1268 = DIRECTION('ref_axis',(0.,0.,1.)) ;
#1269 = DIRECTION('',(-1.,0.,0.)) ;
#1270 = DIRECTION('center_axis',(0.,-0.707106781186545,0.70710678118655)) ;
#1271 = DIRECTION('ref_axis',(0.,-0.70710678118655,-0.707106781186545)) ;
#1272 = DIRECTION('',(-1.,0.,0.)) ;
#1273 = DIRECTION('center_axis',(-1.,0.,0.)) ;
#1274 = DIRECTION('ref_axis',(0.,0.,1.)) ;
#1275 = DIRECTION('center_axis',(-1.,0.,0.)) ;
#1276 = DIRECTION('ref_axis',(0.,0.,1.)) ;
#1277 = DIRECTION('center_axis',(-1.,0.,0.)) ;
#1278 = DIRECTION('ref_axis',(0.,0.,1.)) ;
#1279 = DIRECTION('',(0.,0.,1.)) ;
#1280 = DIRECTION('',(1.,0.,0.)) ;
#1281 = DIRECTION('',(0.,0.,1.)) ;
#1282 = DIRECTION('',(1.,0.,0.)) ;
#1283 = DIRECTION('',(0.,0.,1.)) ;
#1284 = DIRECTION('',(1.,0.,0.)) ;
#1285 = DIRECTION('',(0.,0.165270492834508,0.986248277158566)) ;
#1286 = DIRECTION('',(0.,-0.986248277158566,0.165270492834508)) ;
#1287 = DIRECTION('',(0.,0.,1.)) ;
#1288 = DIRECTION('',(1.,0.,0.)) ;
#1289 = DIRECTION('',(0.,0.587785252292474,0.809016994374947)) ;
#1290 = DIRECTION('',(1.,0.,0.)) ;
#1291 = DIRECTION('',(0.,0.951056516295154,0.309016994374945)) ;
#1292 = DIRECTION('',(1.,0.,0.)) ;
#1293 = DIRECTION('',(0.,0.951056516295152,-0.309016994374952)) ;
#1294 = DIRECTION('',(1.,0.,0.)) ;
#1295 = DIRECTION('',(0.,0.587785252292469,-0.809016994374951)) ;
#1296 = DIRECTION('',(1.,0.,0.)) ;
#1297 = DIRECTION('',(0.,-6.98399671428262E-15,-1.)) ;
#1298 = DIRECTION('',(1.,0.,0.)) ;
#1299 = DIRECTION('',(0.,-0.58778525229248,-0.809016994374942)) ;
#1300 = DIRECTION('',(1.,0.,0.)) ;
#1301 = DIRECTION('',(0.,-0.951056516295157,-0.309016994374938)) ;
#1302 = DIRECTION('',(1.,0.,0.)) ;
#1303 = DIRECTION('',(0.,-0.95105651629515,0.309016994374958)) ;
#1304 = DIRECTION('',(1.,0.,0.)) ;
#1305 = DIRECTION('',(0.,-0.587785252292463,0.809016994374955)) ;
#1306 = DIRECTION('',(1.,0.,0.)) ;
#1307 = CARTESIAN_POINT('',(0.,0.,0.)) ;
#1308 = CARTESIAN_POINT('',(0.,0.,0.)) ;
#1309 = CARTESIAN_POINT('Origin',(0.,42.5000000000009,73.6121593216768)) ;
#1310 = CARTESIAN_POINT('',(-6.35,42.5000000000009,80.1121593216768)) ;
#1311 = CARTESIAN_POINT('Origin',(-6.35,42.5000000000009,73.6121593216768)) ;
#1312 = CARTESIAN_POINT('',(7.59281015471356E-16,42.5000000000009,80.1121593216768)) ;
#1313 = CARTESIAN_POINT('',(0.,42.5000000000009,80.1121593216768)) ;
#1314 = CARTESIAN_POINT('Origin',(7.59281015471356E-16,42.5000000000009,73.6121593216768)) ;
#1315 = CARTESIAN_POINT('Origin',(0.,-42.4999999999993,73.6121593216777)) ;
#1316 = CARTESIAN_POINT('',(-6.35,-42.4999999999993,80.1121593216777)) ;
#1317 = CARTESIAN_POINT('Origin',(-6.35,-42.4999999999993,73.6121593216777)) ;
#1318 = CARTESIAN_POINT('',(7.59281015471356E-16,-42.4999999999993,80.1121593216777)) ;
#1319 = CARTESIAN_POINT('',(0.,-42.4999999999993,80.1121593216777)) ;
#1320 = CARTESIAN_POINT('Origin',(7.59281015471356E-16,-42.4999999999993,
73.6121593216777)) ;
#1321 = CARTESIAN_POINT('Origin',(0.,-85.,0.)) ;
#1322 = CARTESIAN_POINT('',(-6.35,-85.,6.49999999999999)) ;
#1323 = CARTESIAN_POINT('Origin',(-6.35,-85.,0.)) ;
#1324 = CARTESIAN_POINT('',(7.59281015471356E-16,-85.,6.49999999999999)) ;
#1325 = CARTESIAN_POINT('',(0.,-85.,6.49999999999999)) ;
#1326 = CARTESIAN_POINT('Origin',(7.59281015471356E-16,-85.,0.)) ;
#1327 = CARTESIAN_POINT('Origin',(0.,-42.5000000000004,-73.6121593216771)) ;
#1328 = CARTESIAN_POINT('',(-6.35,-42.5000000000004,-67.1121593216771)) ;
#1329 = CARTESIAN_POINT('Origin',(-6.35,-42.5000000000004,-73.6121593216771)) ;
#1330 = CARTESIAN_POINT('',(7.59281015471356E-16,-42.5000000000004,-67.1121593216771)) ;
#1331 = CARTESIAN_POINT('',(0.,-42.5000000000004,-67.1121593216771)) ;
#1332 = CARTESIAN_POINT('Origin',(7.59281015471356E-16,-42.5000000000004,
-73.6121593216771)) ;
#1333 = CARTESIAN_POINT('Origin',(0.,42.4999999999999,-73.6121593216774)) ;
#1334 = CARTESIAN_POINT('',(-6.35,42.4999999999999,-67.1121593216774)) ;
#1335 = CARTESIAN_POINT('Origin',(-6.35,42.4999999999999,-73.6121593216774)) ;
#1336 = CARTESIAN_POINT('',(7.59281015471356E-16,42.4999999999999,-67.1121593216774)) ;
#1337 = CARTESIAN_POINT('',(0.,42.4999999999999,-67.1121593216774)) ;
#1338 = CARTESIAN_POINT('Origin',(7.59281015471356E-16,42.4999999999999,-73.6121593216774)) ;
#1339 = CARTESIAN_POINT('Origin',(0.,85.,0.)) ;
#1340 = CARTESIAN_POINT('',(-6.35,85.,6.49999999999999)) ;
#1341 = CARTESIAN_POINT('Origin',(-6.35,85.,0.)) ;
#1342 = CARTESIAN_POINT('',(7.59281015471356E-16,85.,6.49999999999999)) ;
#1343 = CARTESIAN_POINT('',(0.,85.,6.49999999999999)) ;
#1344 = CARTESIAN_POINT('Origin',(7.59281015471356E-16,85.,0.)) ;
#1345 = CARTESIAN_POINT('Origin',(-6.35,0.,0.)) ;
#1346 = CARTESIAN_POINT('',(-6.35,-4.28626379701574E-15,35.)) ;
#1347 = CARTESIAN_POINT('Origin',(-6.35,0.,0.)) ;
#1348 = CARTESIAN_POINT('',(0.,-4.28626379701574E-15,35.)) ;
#1349 = CARTESIAN_POINT('',(-6.35,-4.28626379701574E-15,35.)) ;
#1350 = CARTESIAN_POINT('Origin',(0.,0.,0.)) ;
#1351 = CARTESIAN_POINT('Origin',(-6.35,0.,0.)) ;
#1352 = CARTESIAN_POINT('',(1.11022302462516E-15,-4.59242549680257E-14,375.)) ;
#1353 = CARTESIAN_POINT('Origin',(0.,0.,0.)) ;
#1354 = CARTESIAN_POINT('',(-6.35,-4.59242549680257E-14,375.)) ;
#1355 = CARTESIAN_POINT('',(-6.35,-4.59242549680257E-14,375.)) ;
#1356 = CARTESIAN_POINT('Origin',(-6.35,0.,0.)) ;
#1357 = CARTESIAN_POINT('Origin',(-6.35,0.,0.)) ;
#1358 = CARTESIAN_POINT('Origin',(0.,0.,0.)) ;
#1359 = CARTESIAN_POINT('',(0.,0.,0.)) ;
#1360 = CARTESIAN_POINT('Origin',(12.,42.5000000000009,-73.6121593216768)) ;
#1361 = CARTESIAN_POINT('',(4.44089209850063E-15,42.5000000000009,-67.1121593216768)) ;
#1362 = CARTESIAN_POINT('Origin',(3.46944695195361E-15,42.5000000000009,-73.6121593216768)) ;
#1363 = CARTESIAN_POINT('',(12.,42.5000000000009,-67.1121593216768)) ;
#1364 = CARTESIAN_POINT('',(12.,42.5000000000009,-67.1121593216768)) ;
#1365 = CARTESIAN_POINT('Origin',(12.,42.5000000000009,-73.6121593216768)) ;
#1366 = CARTESIAN_POINT('Origin',(12.,-42.4999999999993,-73.6121593216777)) ;
#1367 = CARTESIAN_POINT('',(4.44089209850063E-15,-42.4999999999993,-67.1121593216777)) ;
#1368 = CARTESIAN_POINT('Origin',(3.46944695195361E-15,-42.4999999999993,
-73.6121593216777)) ;
#1369 = CARTESIAN_POINT('',(12.,-42.4999999999993,-67.1121593216777)) ;
#1370 = CARTESIAN_POINT('',(12.,-42.4999999999993,-67.1121593216777)) ;
#1371 = CARTESIAN_POINT('Origin',(12.,-42.4999999999993,-73.6121593216777)) ;
#1372 = CARTESIAN_POINT('Origin',(12.,-85.,0.)) ;
#1373 = CARTESIAN_POINT('',(4.44089209850063E-15,-85.,6.49999999999999)) ;
#1374 = CARTESIAN_POINT('Origin',(3.46944695195361E-15,-85.,0.)) ;
#1375 = CARTESIAN_POINT('',(12.,-85.,6.49999999999999)) ;
#1376 = CARTESIAN_POINT('',(12.,-85.,6.49999999999999)) ;
#1377 = CARTESIAN_POINT('Origin',(12.,-85.,0.)) ;
#1378 = CARTESIAN_POINT('Origin',(12.,-42.5000000000003,73.6121593216771)) ;
#1379 = CARTESIAN_POINT('',(4.44089209850063E-15,-42.5000000000003,80.1121593216771)) ;
#1380 = CARTESIAN_POINT('Origin',(3.46944695195361E-15,-42.5000000000003,
73.6121593216771)) ;
#1381 = CARTESIAN_POINT('',(12.,-42.5000000000003,80.1121593216771)) ;
#1382 = CARTESIAN_POINT('',(12.,-42.5000000000003,80.1121593216771)) ;
#1383 = CARTESIAN_POINT('Origin',(12.,-42.5000000000003,73.6121593216771)) ;
#1384 = CARTESIAN_POINT('Origin',(12.,42.4999999999998,73.6121593216774)) ;
#1385 = CARTESIAN_POINT('',(4.44089209850063E-15,42.4999999999998,80.1121593216774)) ;
#1386 = CARTESIAN_POINT('Origin',(3.46944695195361E-15,42.4999999999998,73.6121593216774)) ;
#1387 = CARTESIAN_POINT('',(12.,42.4999999999998,80.1121593216774)) ;
#1388 = CARTESIAN_POINT('',(12.,42.4999999999998,80.1121593216774)) ;
#1389 = CARTESIAN_POINT('Origin',(12.,42.4999999999998,73.6121593216774)) ;
#1390 = CARTESIAN_POINT('Origin',(12.,85.,0.)) ;
#1391 = CARTESIAN_POINT('',(4.44089209850063E-15,85.,6.49999999999999)) ;
#1392 = CARTESIAN_POINT('Origin',(3.46944695195361E-15,85.,0.)) ;
#1393 = CARTESIAN_POINT('',(12.,85.,6.49999999999999)) ;
#1394 = CARTESIAN_POINT('',(12.,85.,6.49999999999999)) ;
#1395 = CARTESIAN_POINT('Origin',(12.,85.,0.)) ;
#1396 = CARTESIAN_POINT('Origin',(12.,0.,0.)) ;
#1397 = CARTESIAN_POINT('',(12.,-4.28626379701574E-15,-35.)) ;
#1398 = CARTESIAN_POINT('Origin',(12.,0.,0.)) ;
#1399 = CARTESIAN_POINT('',(0.,-4.28626379701574E-15,-35.)) ;
#1400 = CARTESIAN_POINT('',(12.,-4.28626379701574E-15,-35.)) ;
#1401 = CARTESIAN_POINT('Origin',(0.,0.,0.)) ;
#1402 = CARTESIAN_POINT('Origin',(12.,0.,0.)) ;
#1403 = CARTESIAN_POINT('',(0.,-1.46957615897682E-14,-120.)) ;
#1404 = CARTESIAN_POINT('Origin',(0.,0.,0.)) ;
#1405 = CARTESIAN_POINT('',(12.,-1.46957615897682E-14,-120.)) ;
#1406 = CARTESIAN_POINT('',(12.,-1.46957615897682E-14,-120.)) ;
#1407 = CARTESIAN_POINT('Origin',(12.,0.,0.)) ;
#1408 = CARTESIAN_POINT('Origin',(12.,0.,0.)) ;
#1409 = CARTESIAN_POINT('Origin',(0.,0.,0.)) ;
#1410 = CARTESIAN_POINT('',(0.,0.,0.)) ;
#1411 = CARTESIAN_POINT('Origin',(0.,137.440607642436,0.)) ;
#1412 = CARTESIAN_POINT('',(-3.56501764721271E-14,125.300844495349,291.105782474981)) ;
#1413 = CARTESIAN_POINT('Origin',(0.,125.300844495349,0.)) ;
#1414 = CARTESIAN_POINT('',(-3.5147363135529E-14,137.440607642436,287.)) ;
#1415 = CARTESIAN_POINT('Origin',(-3.75966567338238E-14,137.440607642436,
307.)) ;
#1416 = CARTESIAN_POINT('Origin',(0.,137.440607642436,0.)) ;
#1417 = CARTESIAN_POINT('Origin',(0.,0.,0.)) ;
#1418 = CARTESIAN_POINT('',(-3.49024337756996E-14,130.,285.)) ;
#1419 = CARTESIAN_POINT('Origin',(0.,130.,0.)) ;
#1420 = CARTESIAN_POINT('',(-4.70622011088264E-14,-3.6985068184911E-14,384.29203539823)) ;
#1421 = CARTESIAN_POINT('',(-4.70622011088264E-14,0.,384.29203539823)) ;
#1422 = CARTESIAN_POINT('Origin',(0.,0.,0.)) ;
#1423 = CARTESIAN_POINT('Origin',(0.,0.,0.)) ;
#1424 = CARTESIAN_POINT('',(-3.49024337756996E-14,150.,285.)) ;
#1425 = CARTESIAN_POINT('Origin',(0.,150.,0.)) ;
#1426 = CARTESIAN_POINT('',(-3.49024337756996E-14,0.,285.)) ;
#1427 = CARTESIAN_POINT('Origin',(0.,150.,0.)) ;
#1428 = CARTESIAN_POINT('',(-3.5147363135529E-14,150.,287.)) ;
#1429 = CARTESIAN_POINT('Origin',(0.,150.,0.)) ;
#1430 = CARTESIAN_POINT('Origin',(-3.50248984556143E-14,150.,286.)) ;
#1431 = CARTESIAN_POINT('Origin',(0.,0.,0.)) ;
#1432 = CARTESIAN_POINT('',(-3.5147363135529E-14,0.,287.)) ;
#1433 = CARTESIAN_POINT('Origin',(0.,130.676418876585,0.)) ;
#1434 = CARTESIAN_POINT('',(-4.7256849134996E-14,1.21397631470872,385.881457150732)) ;
#1435 = CARTESIAN_POINT('Origin',(0.,1.21397631470873,0.)) ;
#1436 = CARTESIAN_POINT('',(-3.5147363135529E-14,130.676418876585,287.)) ;
#1437 = CARTESIAN_POINT('Origin',(0.,0.606988157354366,0.)) ;
#1438 = CARTESIAN_POINT('Origin',(-4.71595251219112E-14,0.606988157354366,
385.086746274481)) ;
#1439 = CARTESIAN_POINT('',(0.,0.,0.)) ;
#1440 = CARTESIAN_POINT('Origin',(0.,0.,0.)) ;
#1441 = CARTESIAN_POINT('',(26.,-5.20474889637625E-15,-42.5)) ;
#1442 = CARTESIAN_POINT('Origin',(26.,0.,0.)) ;
#1443 = CARTESIAN_POINT('',(100.,-5.20474889637625E-15,-42.5)) ;
#1444 = CARTESIAN_POINT('',(0.,-5.20474889637625E-15,-42.5)) ;
#1445 = CARTESIAN_POINT('Origin',(100.,0.,0.)) ;
#1446 = CARTESIAN_POINT('Origin',(0.,0.,0.)) ;
#1447 = CARTESIAN_POINT('',(0.,-4.28626379701574E-15,-35.)) ;
#1448 = CARTESIAN_POINT('Origin',(0.,0.,0.)) ;
#1449 = CARTESIAN_POINT('',(26.,-4.28626379701574E-15,-35.)) ;
#1450 = CARTESIAN_POINT('',(0.,-4.28626379701574E-15,-35.)) ;
#1451 = CARTESIAN_POINT('Origin',(26.,0.,0.)) ;
#1452 = CARTESIAN_POINT('Origin',(0.,0.,0.)) ;
#1453 = CARTESIAN_POINT('',(100.,18.3303027798234,-5.)) ;
#1454 = CARTESIAN_POINT('',(100.,18.3303027798234,5.)) ;
#1455 = CARTESIAN_POINT('Origin',(100.,0.,0.)) ;
#1456 = CARTESIAN_POINT('',(0.,18.3303027798234,-5.)) ;
#1457 = CARTESIAN_POINT('',(0.,18.3303027798234,-5.)) ;
#1458 = CARTESIAN_POINT('',(0.,18.3303027798234,5.)) ;
#1459 = CARTESIAN_POINT('Origin',(0.,0.,0.)) ;
#1460 = CARTESIAN_POINT('',(0.,18.3303027798234,5.)) ;
#1461 = CARTESIAN_POINT('Origin',(0.,19.,0.)) ;
#1462 = CARTESIAN_POINT('',(0.,22.3,-5.)) ;
#1463 = CARTESIAN_POINT('',(0.,22.3,5.)) ;
#1464 = CARTESIAN_POINT('',(0.,22.3,5.)) ;
#1465 = CARTESIAN_POINT('',(0.,22.3,5.)) ;
#1466 = CARTESIAN_POINT('',(0.,22.3,-5.)) ;
#1467 = CARTESIAN_POINT('Origin',(26.,35.,0.)) ;
#1468 = CARTESIAN_POINT('Origin',(100.,42.5,0.)) ;
#1469 = CARTESIAN_POINT('',(100.,22.3,5.)) ;
#1470 = CARTESIAN_POINT('',(100.,22.3,5.)) ;
#1471 = CARTESIAN_POINT('',(100.,22.3,-5.)) ;
#1472 = CARTESIAN_POINT('',(100.,22.3,5.)) ;
#1473 = CARTESIAN_POINT('',(100.,22.3,-5.)) ;
#1474 = CARTESIAN_POINT('Origin',(0.,22.3,5.)) ;
#1475 = CARTESIAN_POINT('',(0.,22.3,5.)) ;
#1476 = CARTESIAN_POINT('Origin',(0.,22.3,5.)) ;
#1477 = CARTESIAN_POINT('',(0.,22.3,-5.)) ;
#1478 = CARTESIAN_POINT('Origin',(0.,22.3,-5.)) ;
#1479 = CARTESIAN_POINT('',(0.,0.,0.)) ;
#1480 = CARTESIAN_POINT('Origin',(85.,250.,5.55111512312578E-14)) ;
#1481 = CARTESIAN_POINT('',(85.,250.,5.55111512312578E-14)) ;
#1482 = CARTESIAN_POINT('',(85.,245.240000000001,-1.11022302462516E-13)) ;
#1483 = CARTESIAN_POINT('',(85.,250.,5.55111512312578E-14)) ;
#1484 = CARTESIAN_POINT('',(85.,176.776695296637,176.776695296638)) ;
#1485 = CARTESIAN_POINT('Origin',(85.,0.,0.)) ;
#1486 = CARTESIAN_POINT('',(85.,173.410867018189,173.41086701819)) ;
#1487 = CARTESIAN_POINT('',(85.,173.410867018189,173.41086701819)) ;
#1488 = CARTESIAN_POINT('Origin',(85.,0.,0.)) ;
#1489 = CARTESIAN_POINT('Origin',(-85.,245.240000000001,-1.11022302462516E-13)) ;
#1490 = CARTESIAN_POINT('',(-85.,245.240000000001,-1.11022302462516E-13)) ;
#1491 = CARTESIAN_POINT('',(-85.,250.,5.55111512312578E-14)) ;
#1492 = CARTESIAN_POINT('',(-85.,245.240000000001,-1.11022302462516E-13)) ;
#1493 = CARTESIAN_POINT('',(-85.,173.410867018189,173.41086701819)) ;
#1494 = CARTESIAN_POINT('Origin',(-85.,0.,0.)) ;
#1495 = CARTESIAN_POINT('',(-85.,176.776695296637,176.776695296638)) ;
#1496 = CARTESIAN_POINT('',(-85.,173.410867018189,173.41086701819)) ;
#1497 = CARTESIAN_POINT('Origin',(-85.,0.,0.)) ;
#1498 = CARTESIAN_POINT('Origin',(85.,245.240000000001,-1.11022302462516E-13)) ;
#1499 = CARTESIAN_POINT('',(-85.,245.24,-50.0000000000003)) ;
#1500 = CARTESIAN_POINT('',(-85.,245.240000000001,-1.11022302462516E-13)) ;
#1501 = CARTESIAN_POINT('',(85.,245.24,-50.0000000000003)) ;
#1502 = CARTESIAN_POINT('',(85.,245.24,-50.0000000000003)) ;
#1503 = CARTESIAN_POINT('',(85.,245.240000000001,-1.11022302462516E-13)) ;
#1504 = CARTESIAN_POINT('',(85.,245.240000000001,-1.11022302462516E-13)) ;
#1505 = CARTESIAN_POINT('Origin',(85.,250.,-50.0000000000002)) ;
#1506 = CARTESIAN_POINT('',(-85.,250.,-50.0000000000002)) ;
#1507 = CARTESIAN_POINT('',(-85.,250.,-50.0000000000002)) ;
#1508 = CARTESIAN_POINT('',(85.,250.,-50.0000000000002)) ;
#1509 = CARTESIAN_POINT('',(85.,250.,-50.0000000000002)) ;
#1510 = CARTESIAN_POINT('',(85.,250.,-50.0000000000002)) ;
#1511 = CARTESIAN_POINT('Origin',(85.,250.,5.55111512312578E-14)) ;
#1512 = CARTESIAN_POINT('',(-85.,250.,5.55111512312578E-14)) ;
#1513 = CARTESIAN_POINT('',(85.,250.,5.55111512312578E-14)) ;
#1514 = CARTESIAN_POINT('',(85.,250.,5.55111512312578E-14)) ;
#1515 = CARTESIAN_POINT('Origin',(85.,0.,0.)) ;
#1516 = CARTESIAN_POINT('',(85.,176.776695296637,176.776695296638)) ;
#1517 = CARTESIAN_POINT('Origin',(85.,173.410867018189,173.41086701819)) ;
#1518 = CARTESIAN_POINT('',(85.,173.410867018189,173.41086701819)) ;
#1519 = CARTESIAN_POINT('Origin',(85.,0.,0.)) ;
#1520 = CARTESIAN_POINT('Origin',(85.,0.,0.)) ;
#1521 = CARTESIAN_POINT('Origin',(-85.,0.,0.)) ;
#1522 = CARTESIAN_POINT('',(868.70645023367,1136.01925527306,1609.99261617346)) ;
#1523 = CARTESIAN_POINT('',(868.70645023367,1136.01925527305,1609.99261617347)) ;
#1524 = CARTESIAN_POINT('',(953.70645023367,1040.77925527306,1328.07642594021)) ;
#1525 = CARTESIAN_POINT('',(1013.82058224513,1136.01925527306,1609.99261617347)) ;
#1526 = CARTESIAN_POINT('',(842.70645023367,1136.01925527305,1609.99261617347)) ;
#1527 = CARTESIAN_POINT('',(953.70645023367,893.262297727203,1437.89829471366)) ;
#1528 = CARTESIAN_POINT('',(953.70645023367,838.470246958351,1613.4543450139)) ;
#1529 = CARTESIAN_POINT('',(953.70645023367,897.331804046892,1787.68813255693)) ;
#1530 = CARTESIAN_POINT('',(953.70645023367,1047.36385481575,1894.04827248994)) ;
#1531 = CARTESIAN_POINT('',(953.70645023367,1231.25925527306,1891.90880640671)) ;
#1532 = CARTESIAN_POINT('',(953.70645023367,1378.77621281891,1782.08693763327)) ;
#1533 = CARTESIAN_POINT('',(953.70645023367,1433.56826358776,1606.53088733303)) ;
#1534 = CARTESIAN_POINT('',(953.70645023367,1374.70670649922,1432.29709979)) ;
#1535 = CARTESIAN_POINT('',(953.70645023367,1224.67465573037,1325.93695985699)) ;
#1536 = UNCERTAINTY_MEASURE_WITH_UNIT(LENGTH_MEASURE(0.01),#1550,
'DISTANCE_ACCURACY_VALUE',
'Maximum model space distance between geometric entities at asserted c
onnectivities') ;
#1537 = UNCERTAINTY_MEASURE_WITH_UNIT(LENGTH_MEASURE(0.01),#1550,
'DISTANCE_ACCURACY_VALUE',
'Maximum model space distance between geometric entities at asserted c
onnectivities') ;
#1538 = UNCERTAINTY_MEASURE_WITH_UNIT(LENGTH_MEASURE(0.01),#1550,
'DISTANCE_ACCURACY_VALUE',
'Maximum model space distance between geometric entities at asserted c
onnectivities') ;
#1539 = UNCERTAINTY_MEASURE_WITH_UNIT(LENGTH_MEASURE(0.01),#1550,
'DISTANCE_ACCURACY_VALUE',
'Maximum model space distance between geometric entities at asserted c
onnectivities') ;
#1540 = UNCERTAINTY_MEASURE_WITH_UNIT(LENGTH_MEASURE(0.01),#1550,
'DISTANCE_ACCURACY_VALUE',
'Maximum model space distance between geometric entities at asserted c
onnectivities') ;
#1541 = UNCERTAINTY_MEASURE_WITH_UNIT(LENGTH_MEASURE(0.01),#1550,
'DISTANCE_ACCURACY_VALUE',
'Maximum model space distance between geometric entities at asserted c
onnectivities') ;
#1542 = UNCERTAINTY_MEASURE_WITH_UNIT(LENGTH_MEASURE(0.01),#1550,
'DISTANCE_ACCURACY_VALUE',
'Maximum model space distance between geometric entities at asserted c
onnectivities') ;
#1543 = (
GEOMETRIC_REPRESENTATION_CONTEXT(3)
GLOBAL_UNCERTAINTY_ASSIGNED_CONTEXT((#1536))
GLOBAL_UNIT_ASSIGNED_CONTEXT((#1550,#1552,#1553))
REPRESENTATION_CONTEXT('','3D')
) ;
#1544 = (
GEOMETRIC_REPRESENTATION_CONTEXT(3)
GLOBAL_UNCERTAINTY_ASSIGNED_CONTEXT((#1537))
GLOBAL_UNIT_ASSIGNED_CONTEXT((#1550,#1552,#1553))
REPRESENTATION_CONTEXT('','3D')
) ;
#1545 = (
GEOMETRIC_REPRESENTATION_CONTEXT(3)
GLOBAL_UNCERTAINTY_ASSIGNED_CONTEXT((#1538))
GLOBAL_UNIT_ASSIGNED_CONTEXT((#1550,#1552,#1553))
REPRESENTATION_CONTEXT('','3D')
) ;
#1546 = (
GEOMETRIC_REPRESENTATION_CONTEXT(3)
GLOBAL_UNCERTAINTY_ASSIGNED_CONTEXT((#1539))
GLOBAL_UNIT_ASSIGNED_CONTEXT((#1550,#1552,#1553))
REPRESENTATION_CONTEXT('','3D')
) ;
#1547 = (
GEOMETRIC_REPRESENTATION_CONTEXT(3)
GLOBAL_UNCERTAINTY_ASSIGNED_CONTEXT((#1540))
GLOBAL_UNIT_ASSIGNED_CONTEXT((#1550,#1552,#1553))
REPRESENTATION_CONTEXT('','3D')
) ;
#1548 = (
GEOMETRIC_REPRESENTATION_CONTEXT(3)
GLOBAL_UNCERTAINTY_ASSIGNED_CONTEXT((#1541))
GLOBAL_UNIT_ASSIGNED_CONTEXT((#1550,#1552,#1553))
REPRESENTATION_CONTEXT('','3D')
) ;
#1549 = (
GEOMETRIC_REPRESENTATION_CONTEXT(3)
GLOBAL_UNCERTAINTY_ASSIGNED_CONTEXT((#1542))
GLOBAL_UNIT_ASSIGNED_CONTEXT((#1550,#1552,#1553))
REPRESENTATION_CONTEXT('','3D')
) ;
#1550 = (
LENGTH_UNIT()
NAMED_UNIT(*)
SI_UNIT(.MILLI.,.METRE.)
) ;
#1551 = (
LENGTH_UNIT()
NAMED_UNIT(*)
SI_UNIT($,.METRE.)
) ;
#1552 = (
NAMED_UNIT(*)
PLANE_ANGLE_UNIT()
SI_UNIT($,.RADIAN.)
) ;
#1553 = (
NAMED_UNIT(*)
SI_UNIT($,.STERADIAN.)
SOLID_ANGLE_UNIT()
) ;
#1554 = SHAPE_DEFINITION_REPRESENTATION(#1560,#1580) ;
#1555 = SHAPE_DEFINITION_REPRESENTATION(#1561,#1581) ;
#1556 = SHAPE_DEFINITION_REPRESENTATION(#1562,#1582) ;
#1557 = SHAPE_DEFINITION_REPRESENTATION(#1563,#1583) ;
#1558 = SHAPE_DEFINITION_REPRESENTATION(#1564,#1584) ;
#1559 = SHAPE_DEFINITION_REPRESENTATION(#1565,#1585) ;
#1560 = PRODUCT_DEFINITION_SHAPE('',$,#1587) ;
#1561 = PRODUCT_DEFINITION_SHAPE('',$,#1588) ;
#1562 = PRODUCT_DEFINITION_SHAPE('',$,#1589) ;
#1563 = PRODUCT_DEFINITION_SHAPE('',$,#1590) ;
#1564 = PRODUCT_DEFINITION_SHAPE('',$,#1591) ;
#1565 = PRODUCT_DEFINITION_SHAPE('',$,#1592) ;
#1566 = PRODUCT_DEFINITION_SHAPE($,$,#53) ;
#1567 = PRODUCT_DEFINITION_SHAPE($,$,#54) ;
#1568 = PRODUCT_DEFINITION_SHAPE($,$,#55) ;
#1569 = PRODUCT_DEFINITION_SHAPE($,$,#56) ;
#1570 = PRODUCT_DEFINITION_SHAPE($,$,#57) ;
#1571 = PRODUCT_DEFINITION_SHAPE($,$,#58) ;
#1572 = PRODUCT_DEFINITION_SHAPE($,$,#59) ;
#1573 = PRODUCT_DEFINITION_SHAPE($,$,#60) ;
#1574 = PRODUCT_DEFINITION_SHAPE($,$,#61) ;
#1575 = PRODUCT_DEFINITION_SHAPE($,$,#62) ;
#1576 = PRODUCT_DEFINITION_SHAPE($,$,#63) ;
#1577 = PRODUCT_DEFINITION_SHAPE($,$,#64) ;
#1578 = PRODUCT_DEFINITION_SHAPE($,$,#65) ;
#1579 = PRODUCT_DEFINITION_SHAPE($,$,#66) ;
#1580 = SHAPE_REPRESENTATION('',(#905,#1009,#1010,#1011,#1012,#1013,#1014,
#1015,#1016,#1017,#1018,#1019,#1020,#1021,#1022),#1543) ;
#1581 = SHAPE_REPRESENTATION('',(#906),#1544) ;
#1582 = SHAPE_REPRESENTATION('',(#933),#1545) ;
#1583 = SHAPE_REPRESENTATION('',(#960),#1546) ;
#1584 = SHAPE_REPRESENTATION('',(#978),#1547) ;
#1585 = SHAPE_REPRESENTATION('',(#994),#1548) ;
#1586 = PRODUCT_DEFINITION_CONTEXT('part definition',#1606,'design') ;
#1587 = PRODUCT_DEFINITION('MAS-647','MAS-647',#1593,#1586) ;
#1588 = PRODUCT_DEFINITION('Base_Plate','Base_Plate',#1594,#1586) ;
#1589 = PRODUCT_DEFINITION('Hub_Plate','Hub_Plate',#1595,#1586) ;
#1590 = PRODUCT_DEFINITION('Top_Plate','Top_Plate',#1596,#1586) ;
#1591 = PRODUCT_DEFINITION('Hub','Hub',#1597,#1586) ;
#1592 = PRODUCT_DEFINITION('Blade','Blade',#1598,#1586) ;
#1593 = PRODUCT_DEFINITION_FORMATION('',$,#1608) ;
#1594 = PRODUCT_DEFINITION_FORMATION('',$,#1609) ;
#1595 = PRODUCT_DEFINITION_FORMATION('',$,#1610) ;
#1596 = PRODUCT_DEFINITION_FORMATION('',$,#1611) ;
#1597 = PRODUCT_DEFINITION_FORMATION('',$,#1612) ;
#1598 = PRODUCT_DEFINITION_FORMATION('',$,#1613) ;
#1599 = PRODUCT_RELATED_PRODUCT_CATEGORY('MAS-647','MAS-647',(#1608)) ;
#1600 = PRODUCT_RELATED_PRODUCT_CATEGORY('Base_Plate','Base_Plate',(#1609)) ;
#1601 = PRODUCT_RELATED_PRODUCT_CATEGORY('Hub_Plate','Hub_Plate',(#1610)) ;
#1602 = PRODUCT_RELATED_PRODUCT_CATEGORY('Top_Plate','Top_Plate',(#1611)) ;
#1603 = PRODUCT_RELATED_PRODUCT_CATEGORY('Hub','Hub',(#1612)) ;
#1604 = PRODUCT_RELATED_PRODUCT_CATEGORY('Blade','Blade',(#1613)) ;
#1605 = APPLICATION_PROTOCOL_DEFINITION('international standard',
'automotive_design',2009,#1606) ;
#1606 = APPLICATION_CONTEXT(
'Core Data for Automotive Mechanical Design Process') ;
#1607 = PRODUCT_CONTEXT('part definition',#1606,'mechanical') ;
#1608 = PRODUCT('MAS-647','MAS-647',$,(#1607)) ;
#1609 = PRODUCT('Base_Plate','Base_Plate',$,(#1607)) ;
#1610 = PRODUCT('Hub_Plate','Hub_Plate',$,(#1607)) ;
#1611 = PRODUCT('Top_Plate','Top_Plate',$,(#1607)) ;
#1612 = PRODUCT('Hub','Hub',$,(#1607)) ;
#1613 = PRODUCT('Blade','Blade',$,(#1607)) ;
#1614 = PRESENTATION_STYLE_ASSIGNMENT((#1616)) ;
#1615 = PRESENTATION_STYLE_ASSIGNMENT((#1617)) ;
#1616 = SURFACE_STYLE_USAGE(.BOTH.,#1618) ;
#1617 = SURFACE_STYLE_USAGE(.BOTH.,#1619) ;
#1618 = SURFACE_SIDE_STYLE('',(#1620)) ;
#1619 = SURFACE_SIDE_STYLE('',(#1621)) ;
#1620 = SURFACE_STYLE_FILL_AREA(#1622) ;
#1621 = SURFACE_STYLE_FILL_AREA(#1623) ;
#1622 = FILL_AREA_STYLE('Steel - Satin',(#1624)) ;
#1623 = FILL_AREA_STYLE('Opaque(202,209,238)',(#1625)) ;
#1624 = FILL_AREA_STYLE_COLOUR('Steel - Satin',#1626) ;
#1625 = FILL_AREA_STYLE_COLOUR('Opaque(202,209,238)',#1627) ;
#1626 = COLOUR_RGB('Steel - Satin', 0.09019608, 0.27058824, 0.51372549) ;
#1627 = COLOUR_RGB('Opaque(202,209,238)', 0.09019608, 0.27058824, 0.51372549) ;
ENDSEC;
END-ISO-10303-21;
